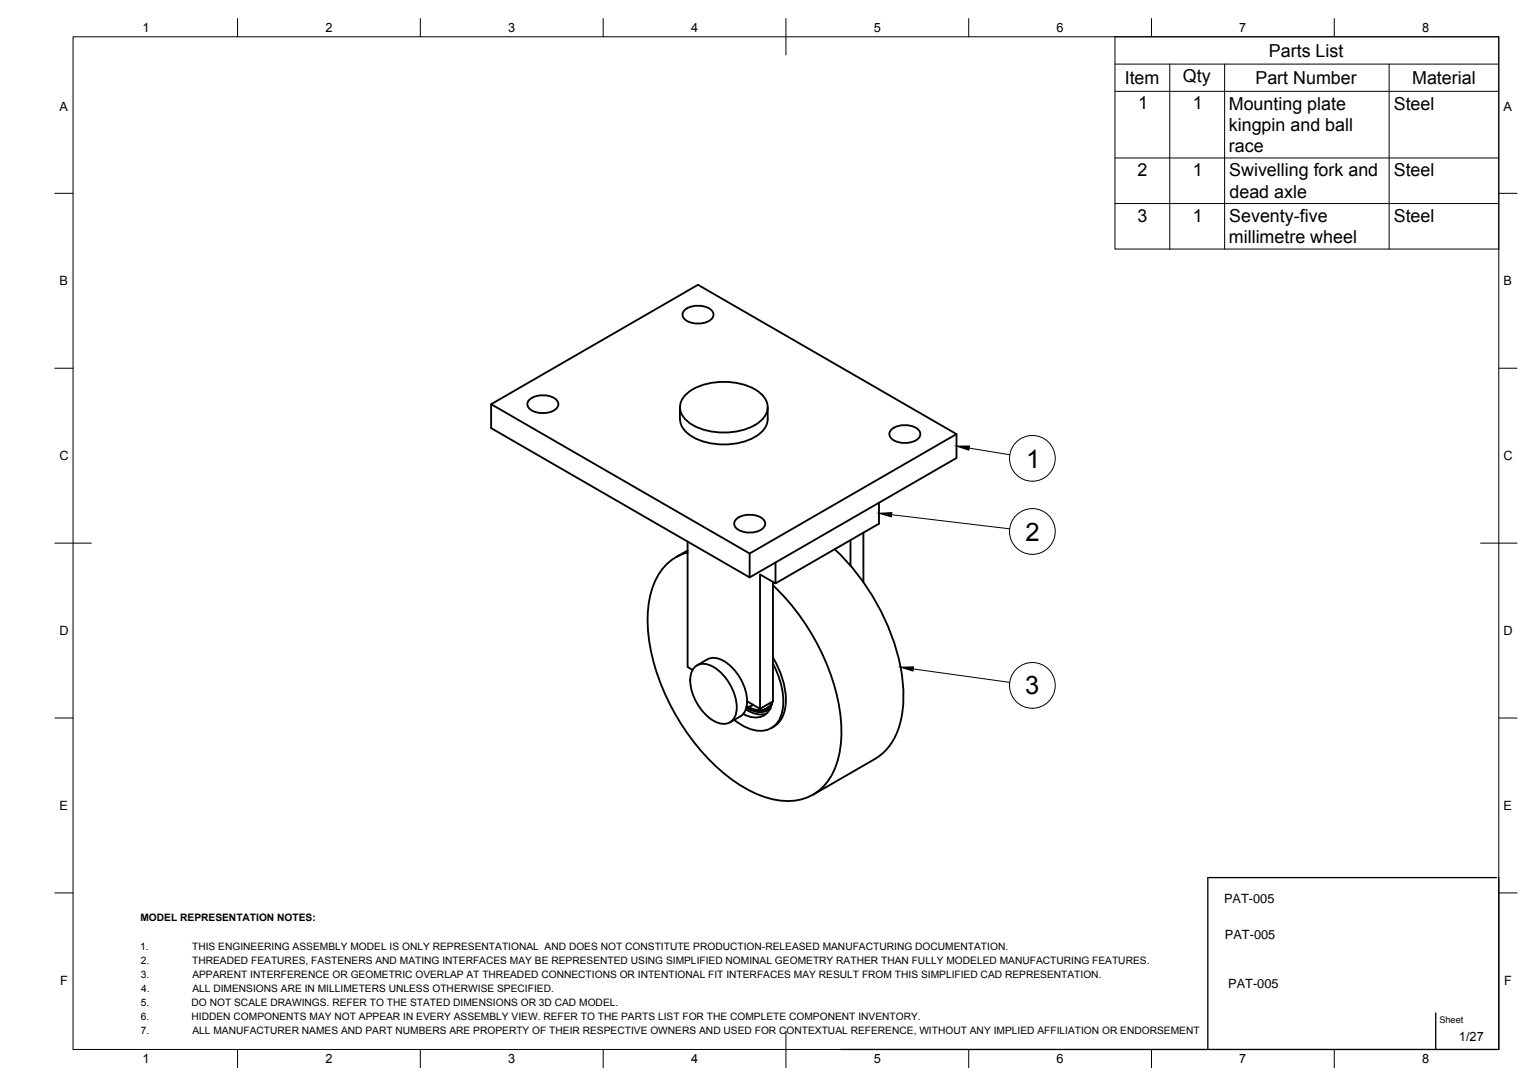
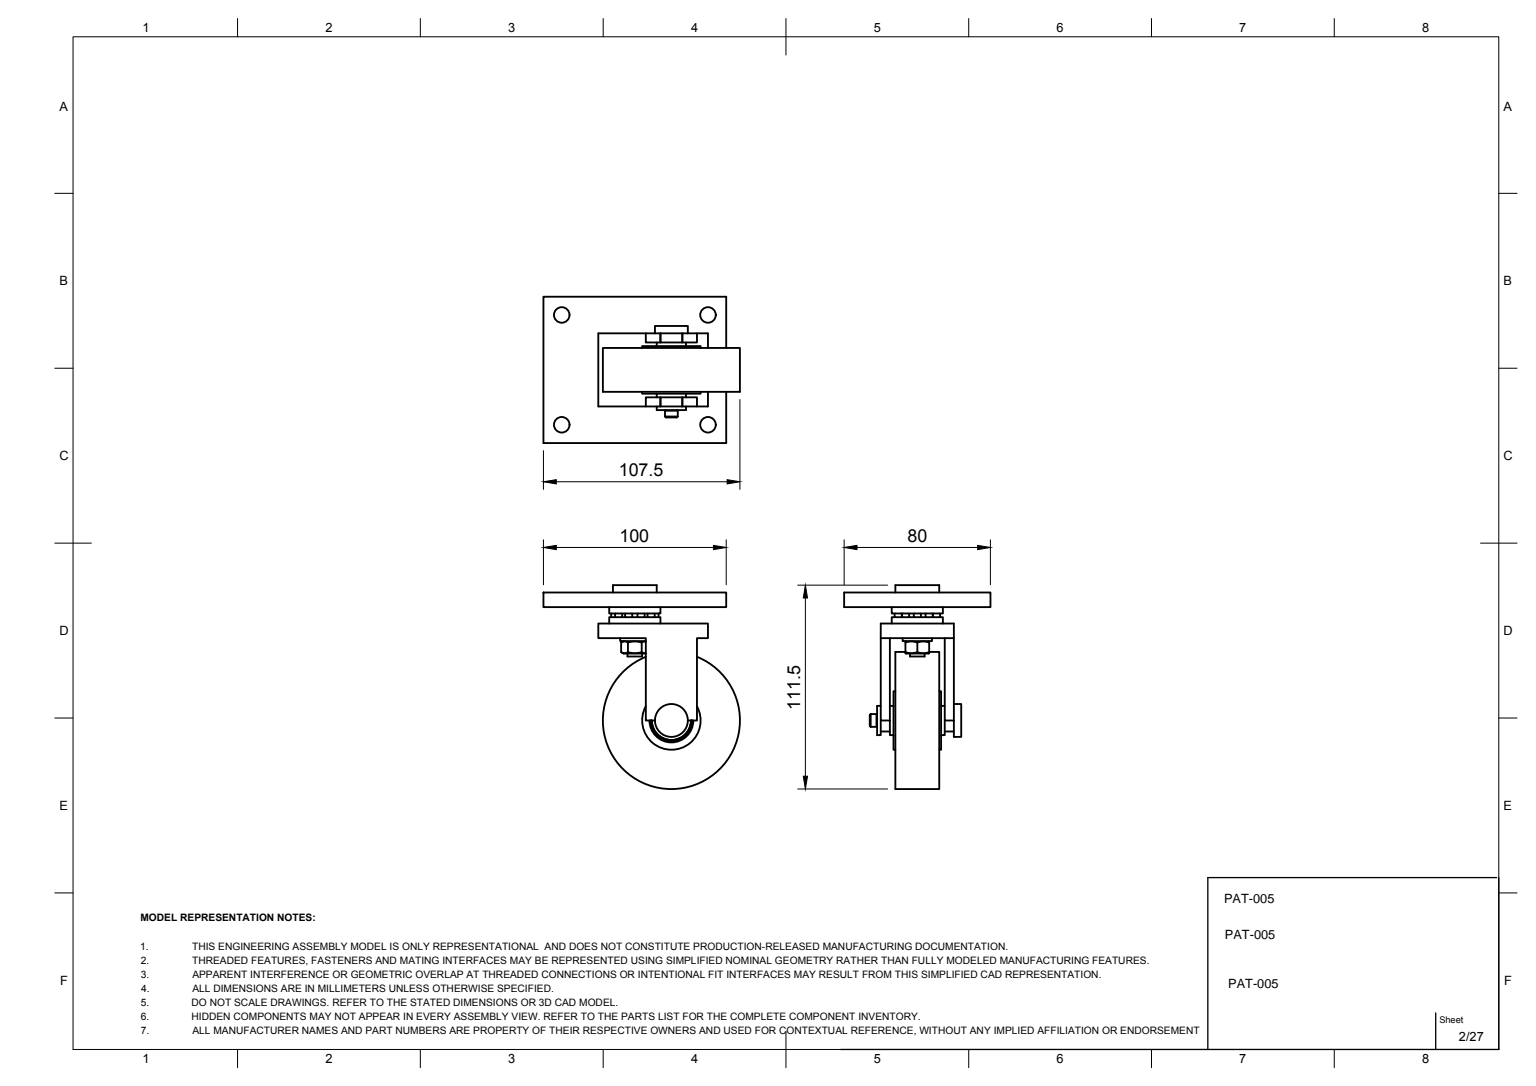
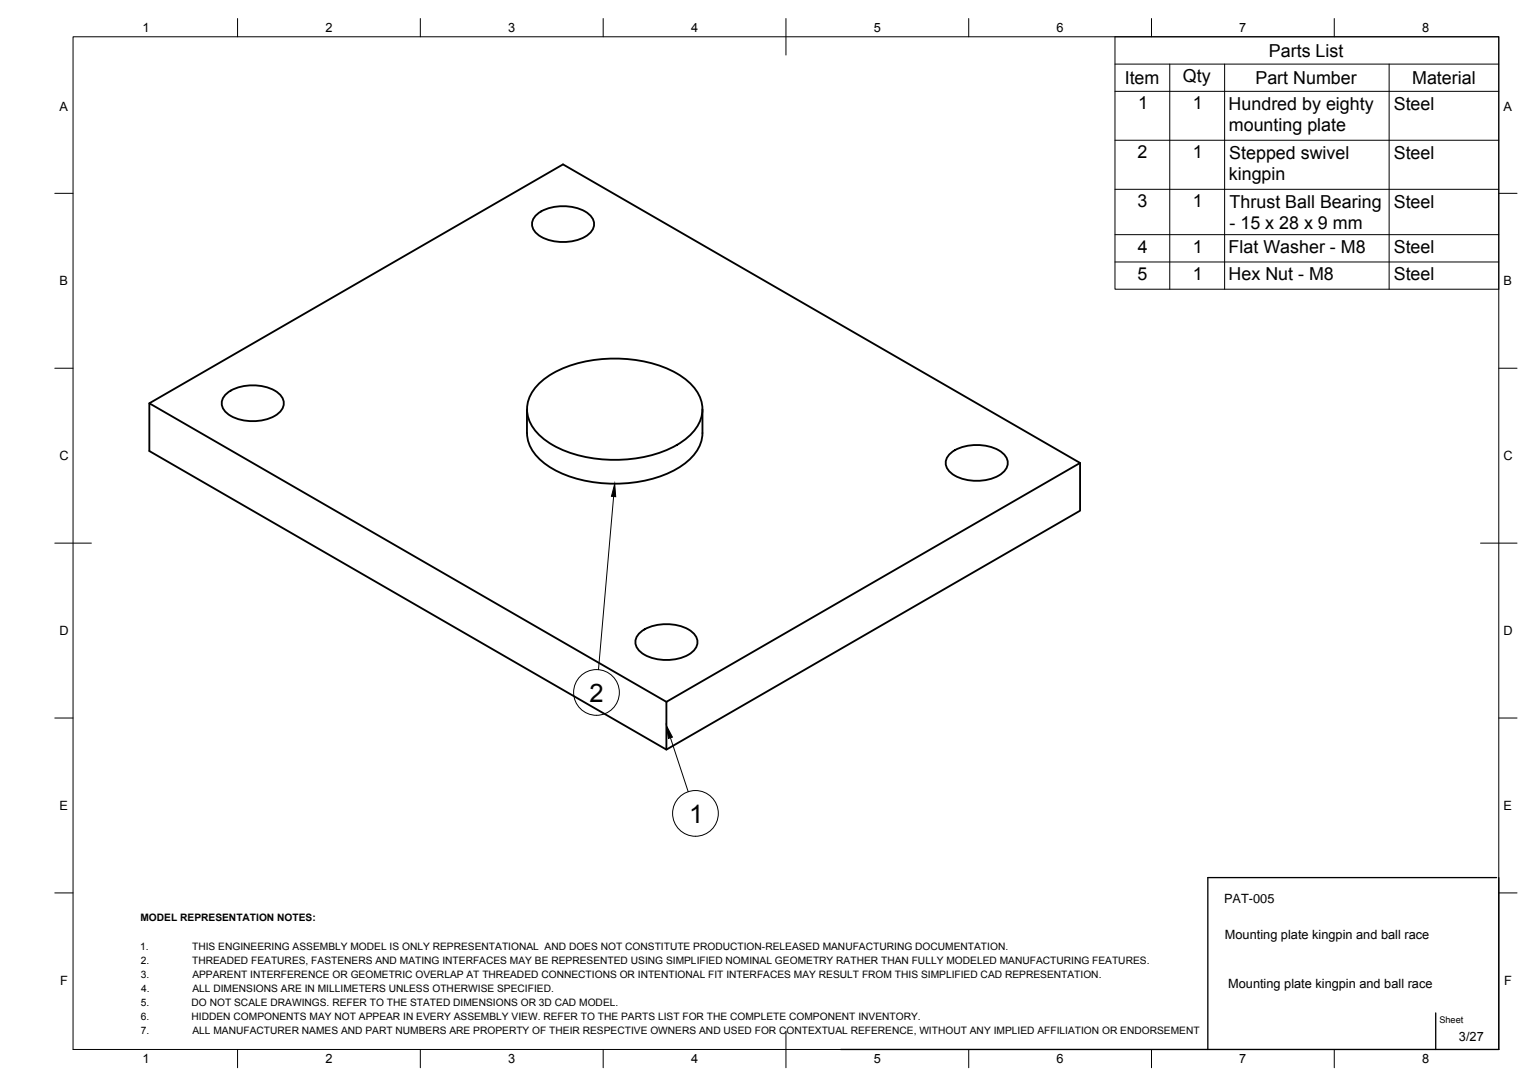
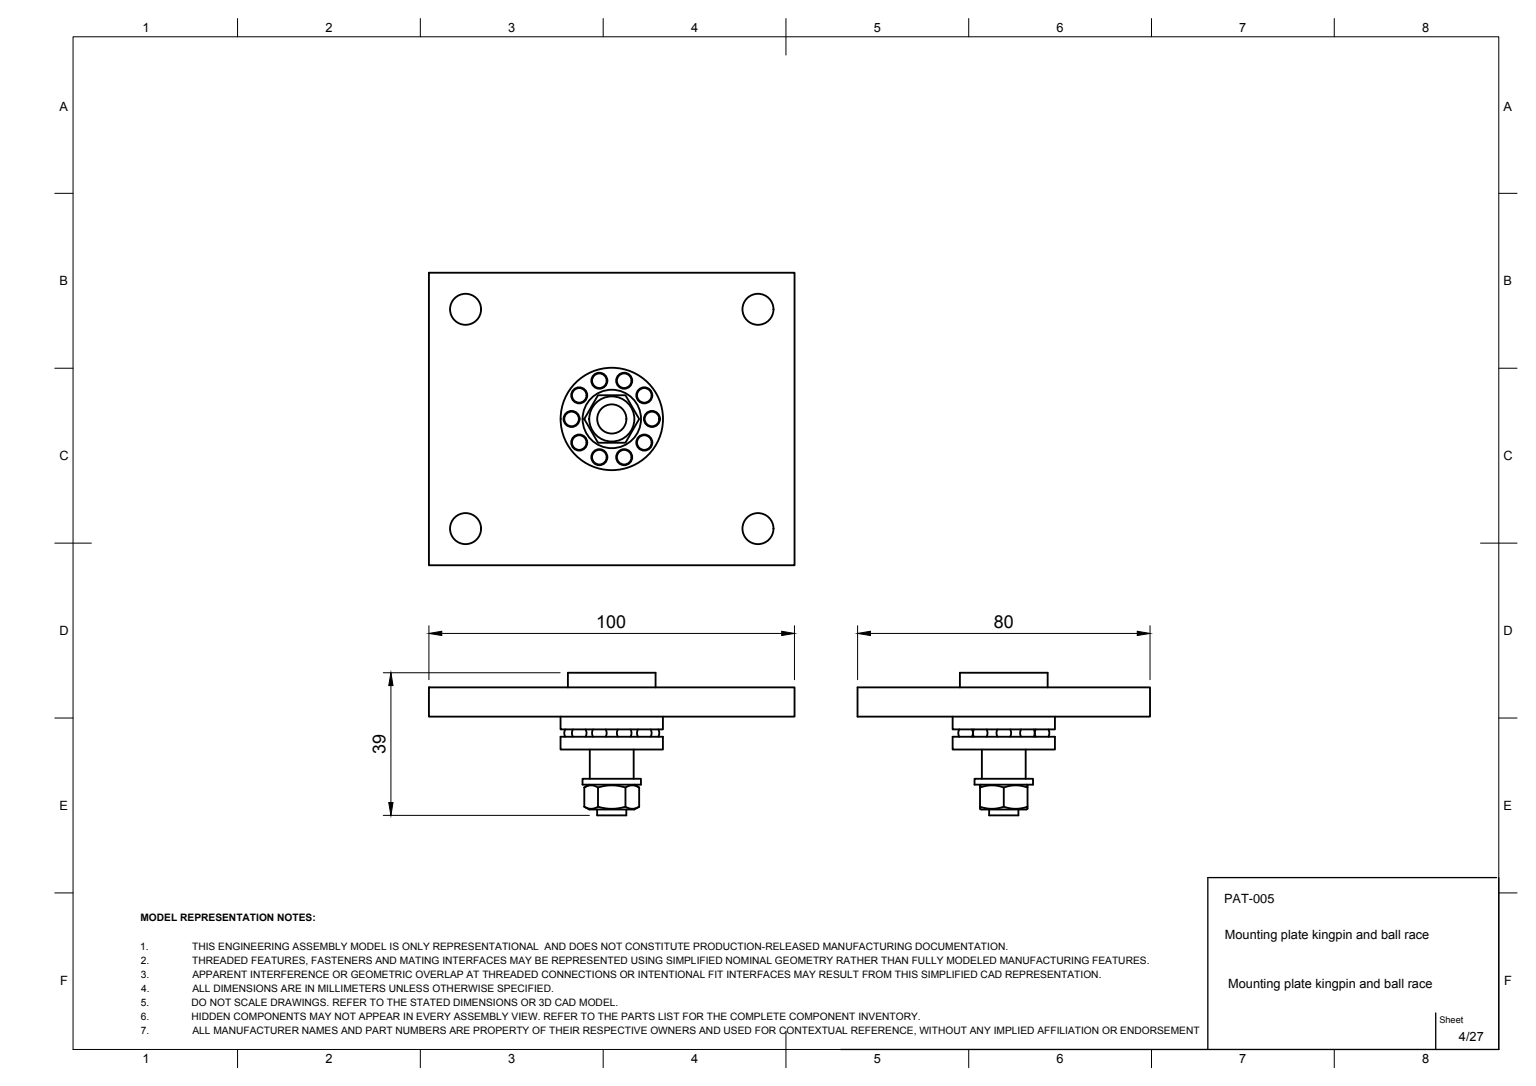
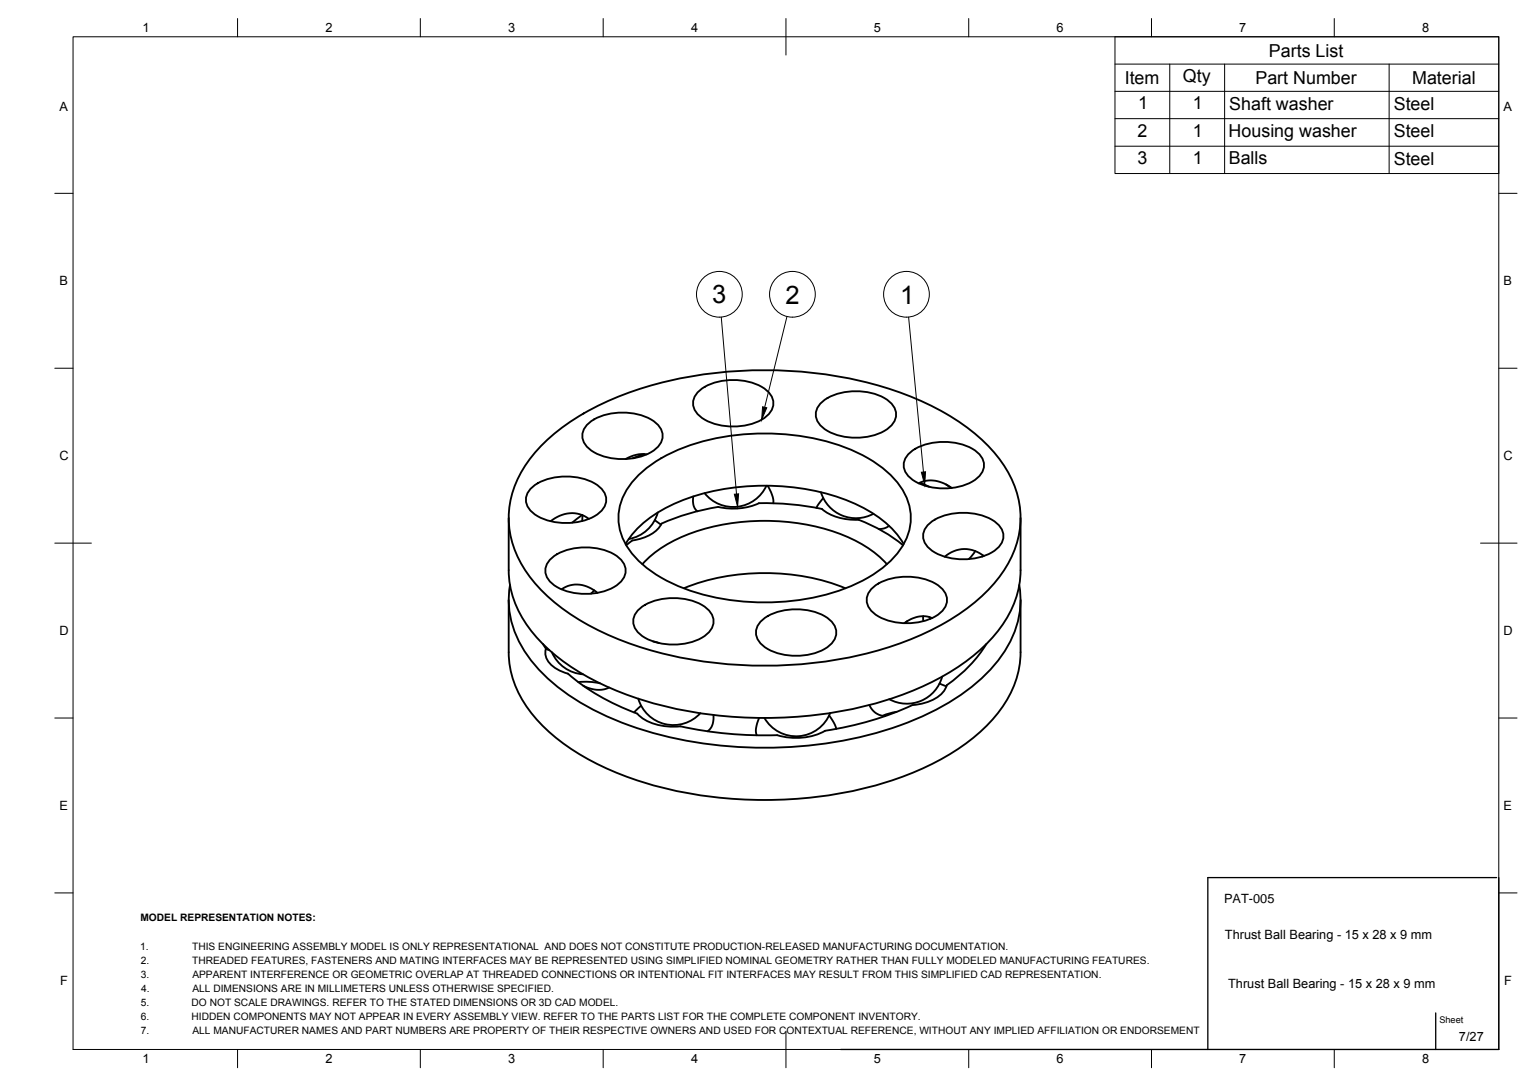
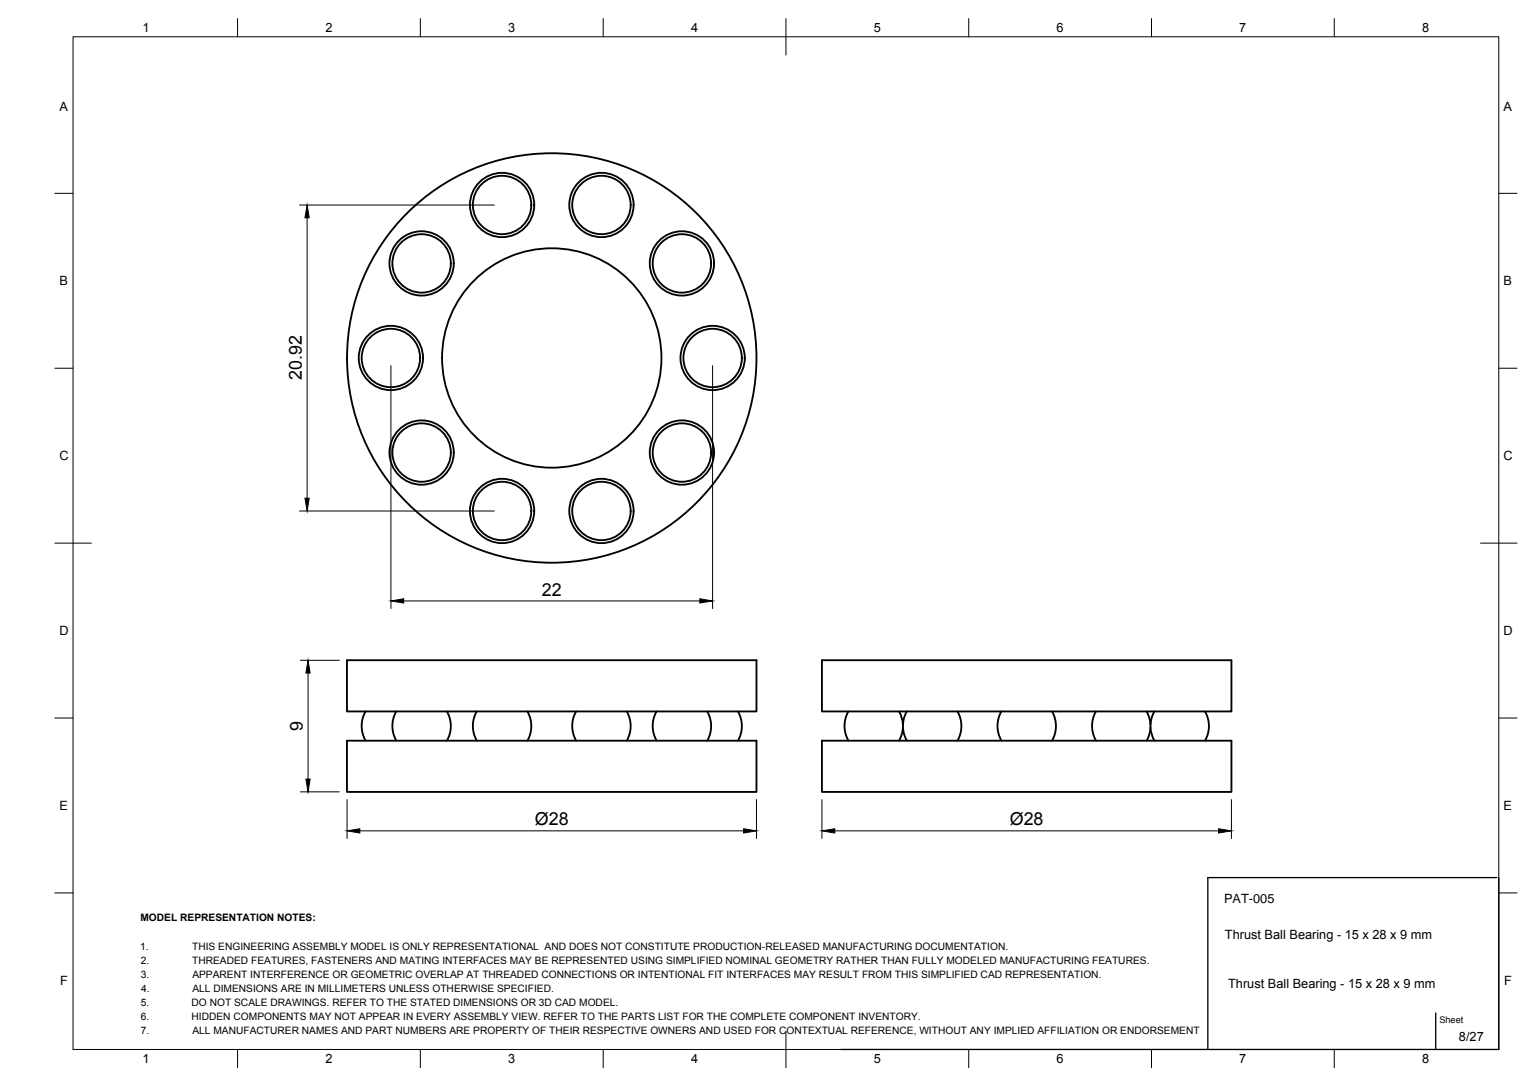
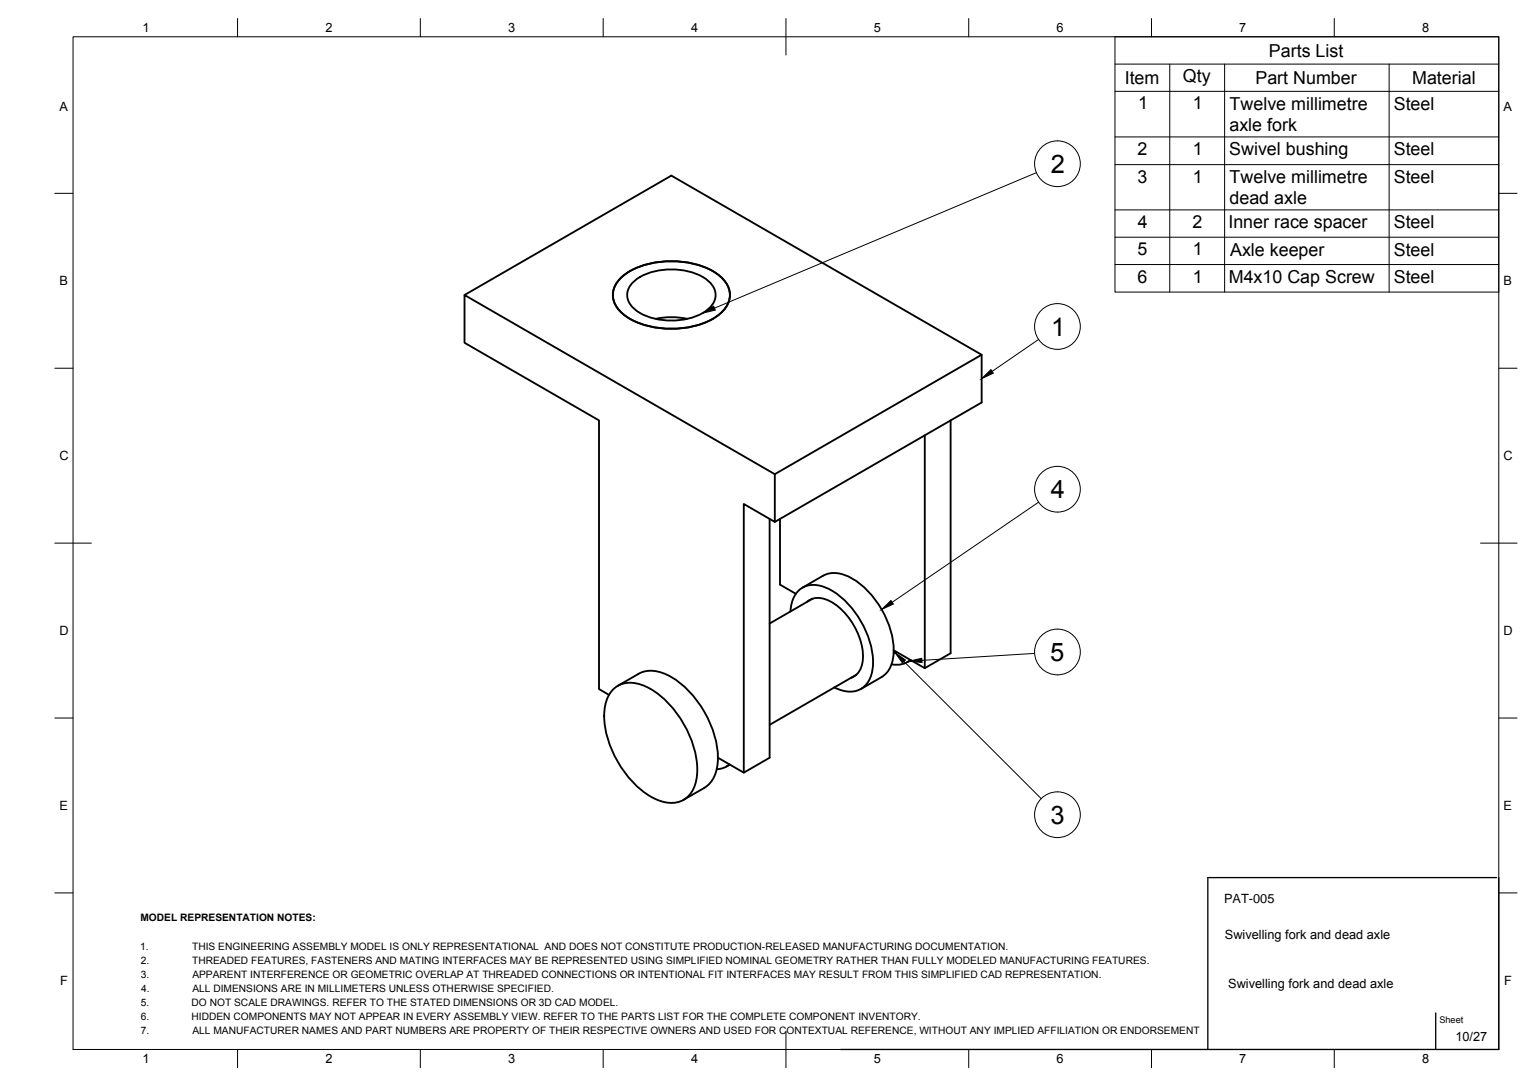
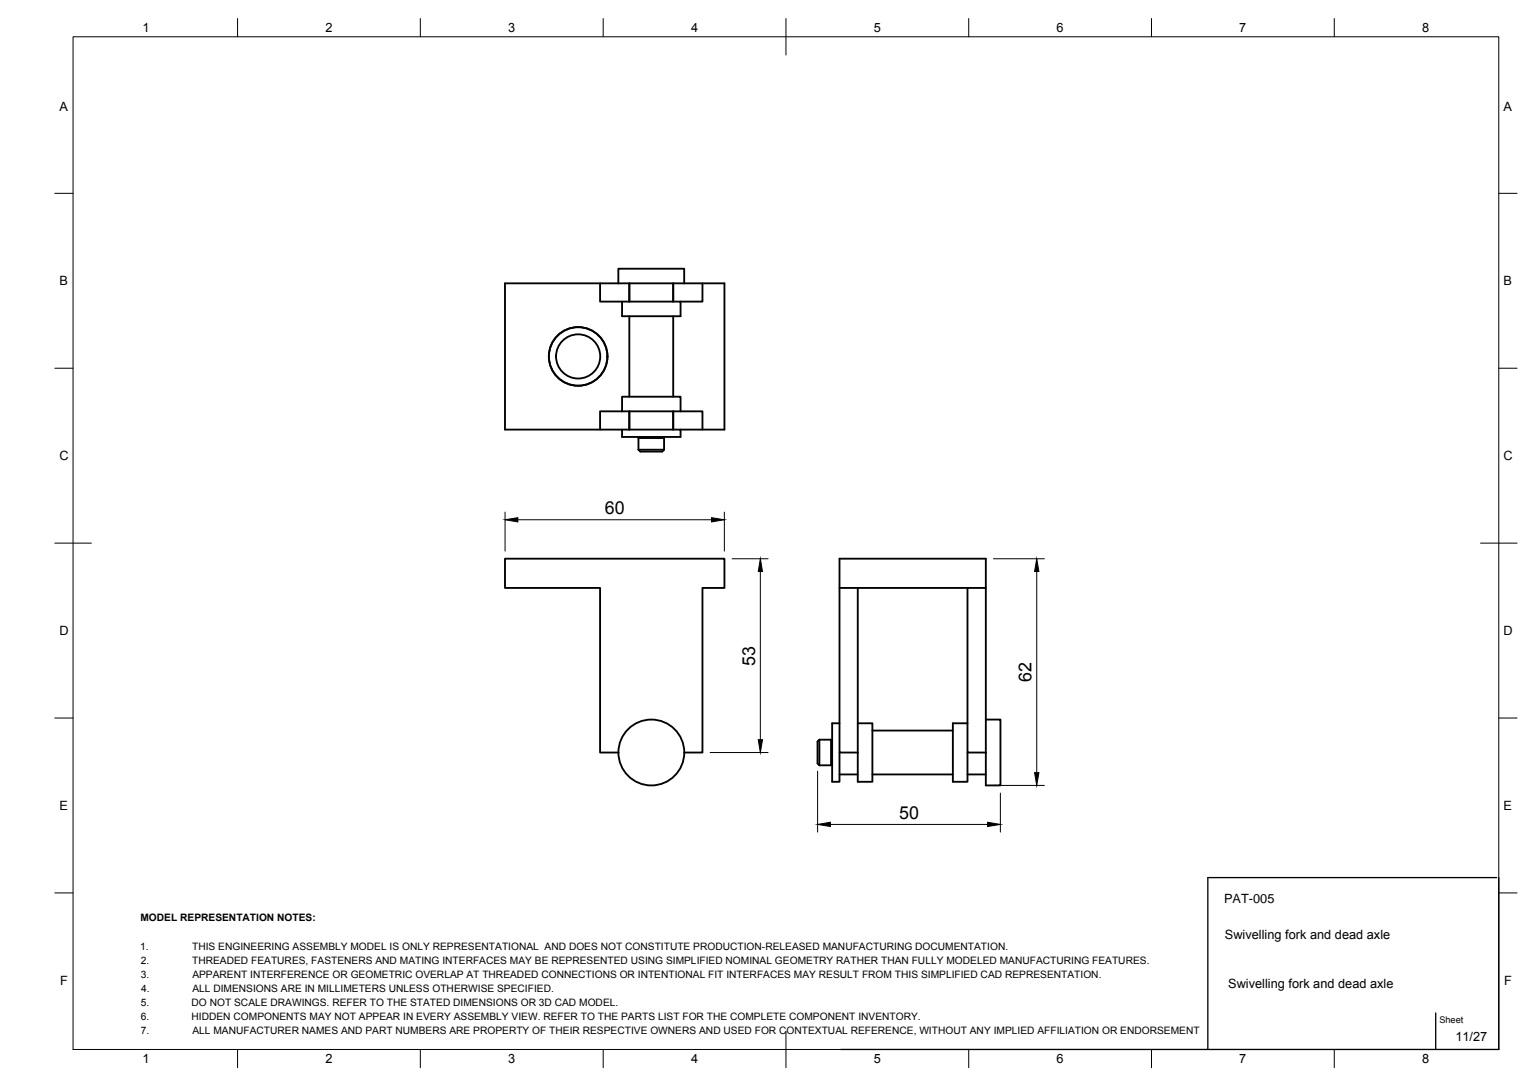
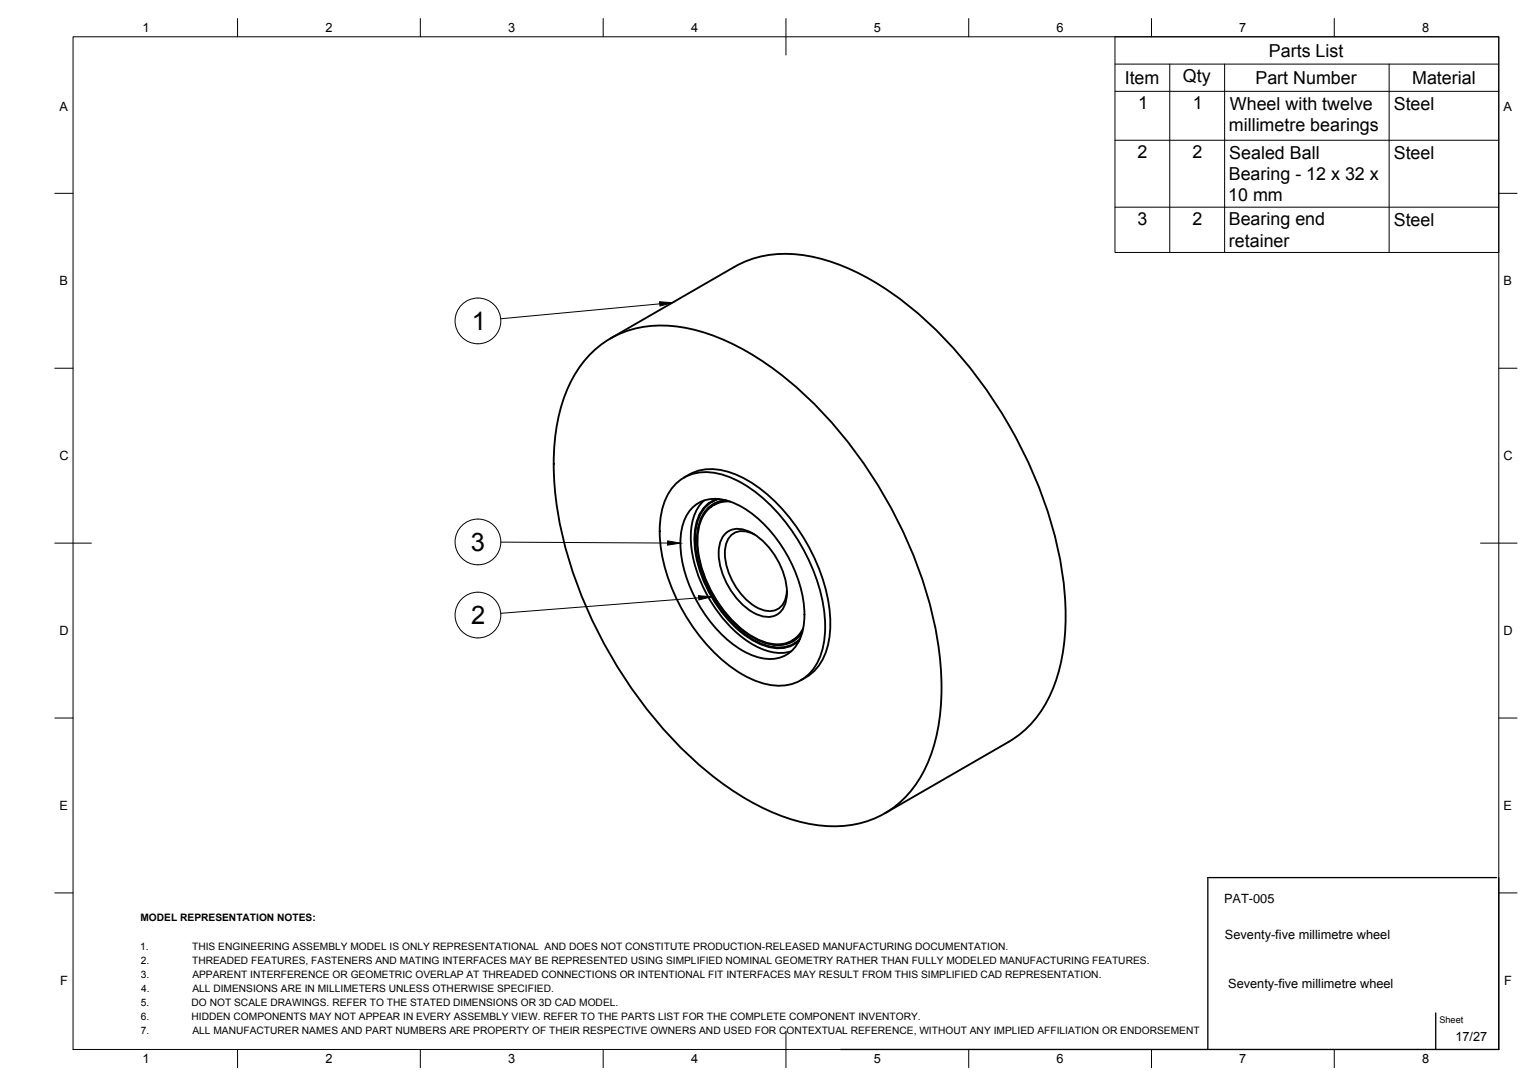
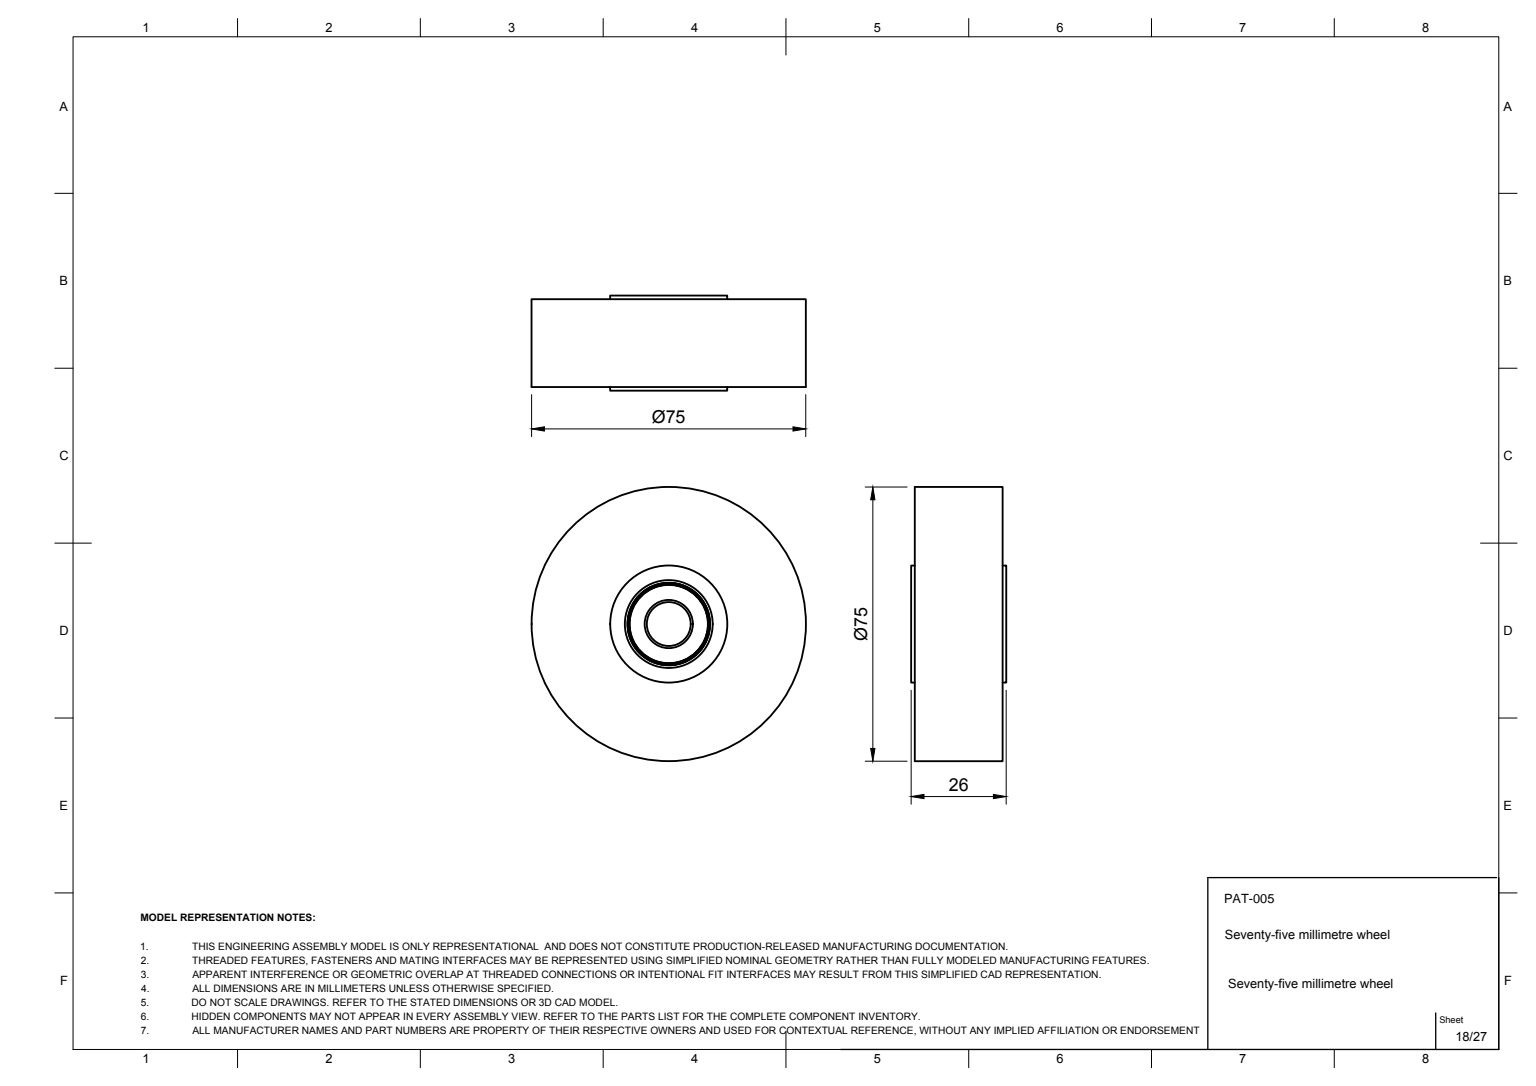
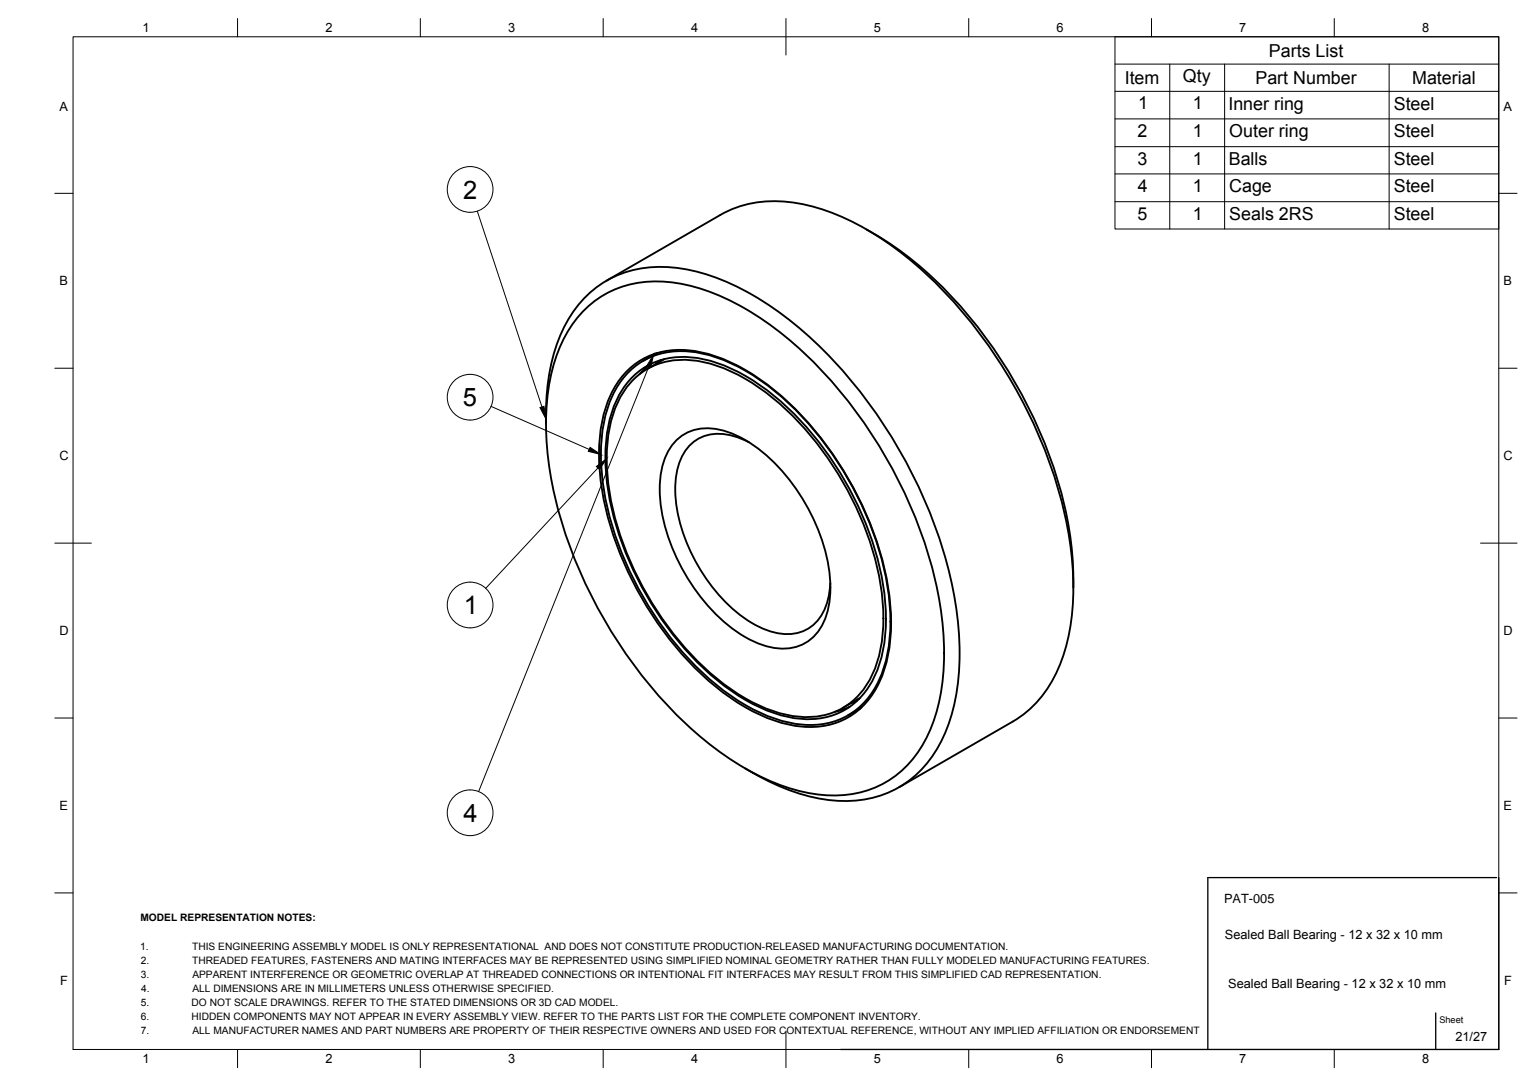
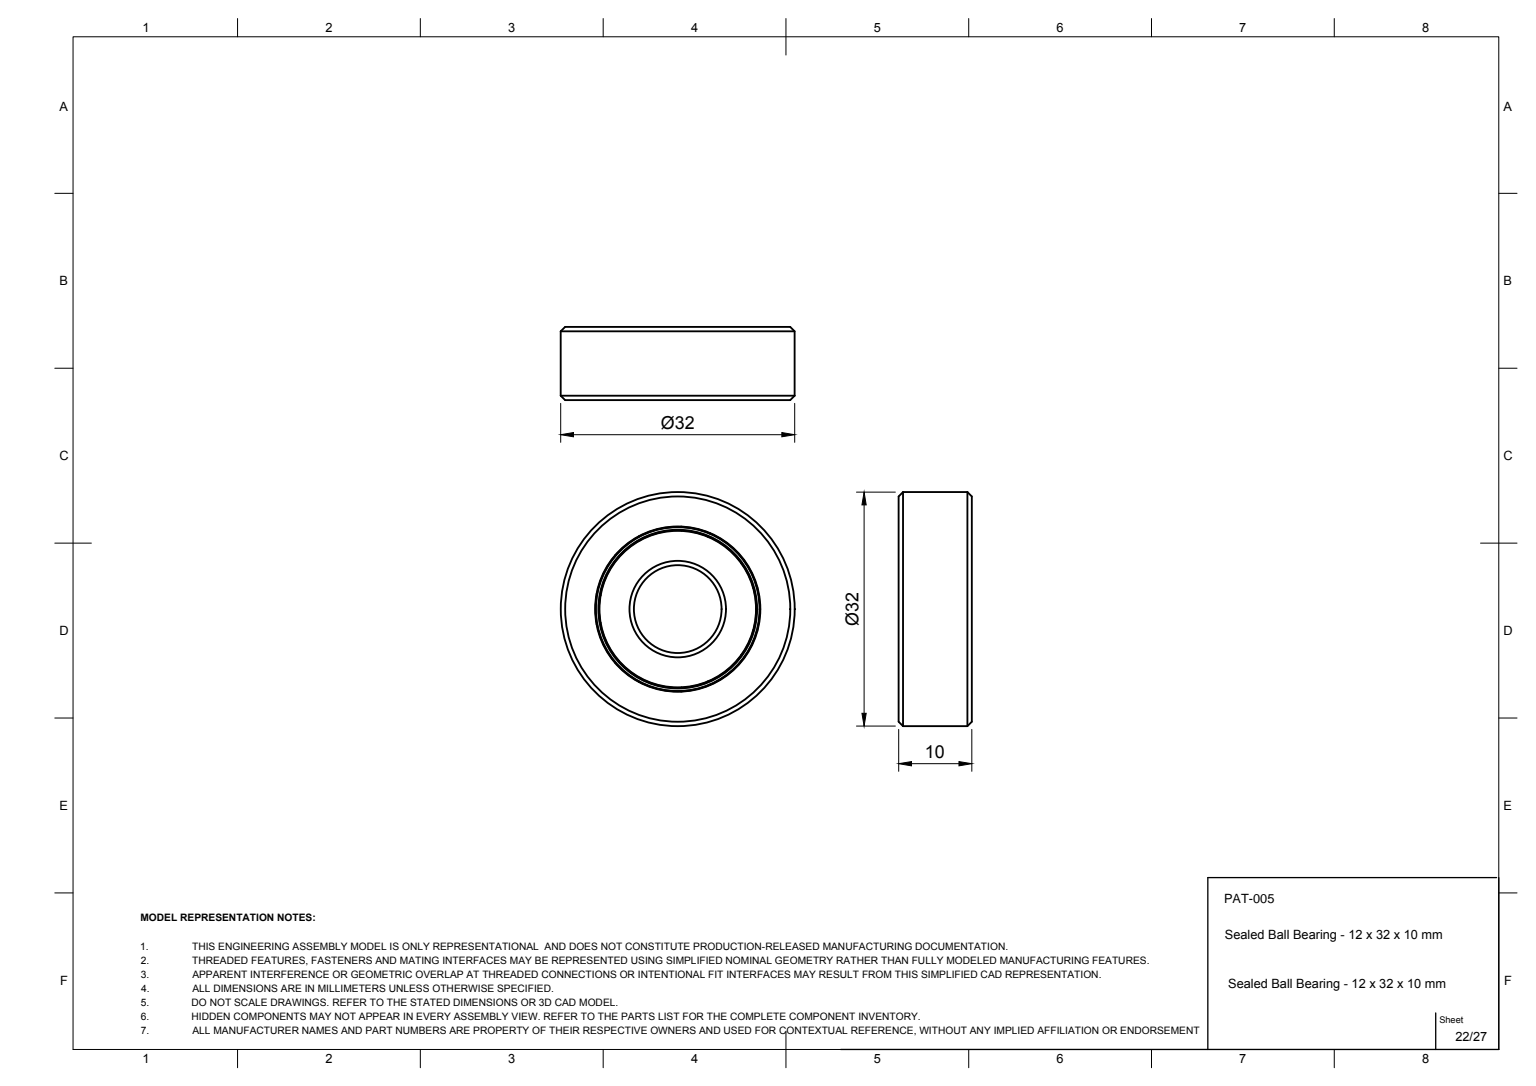
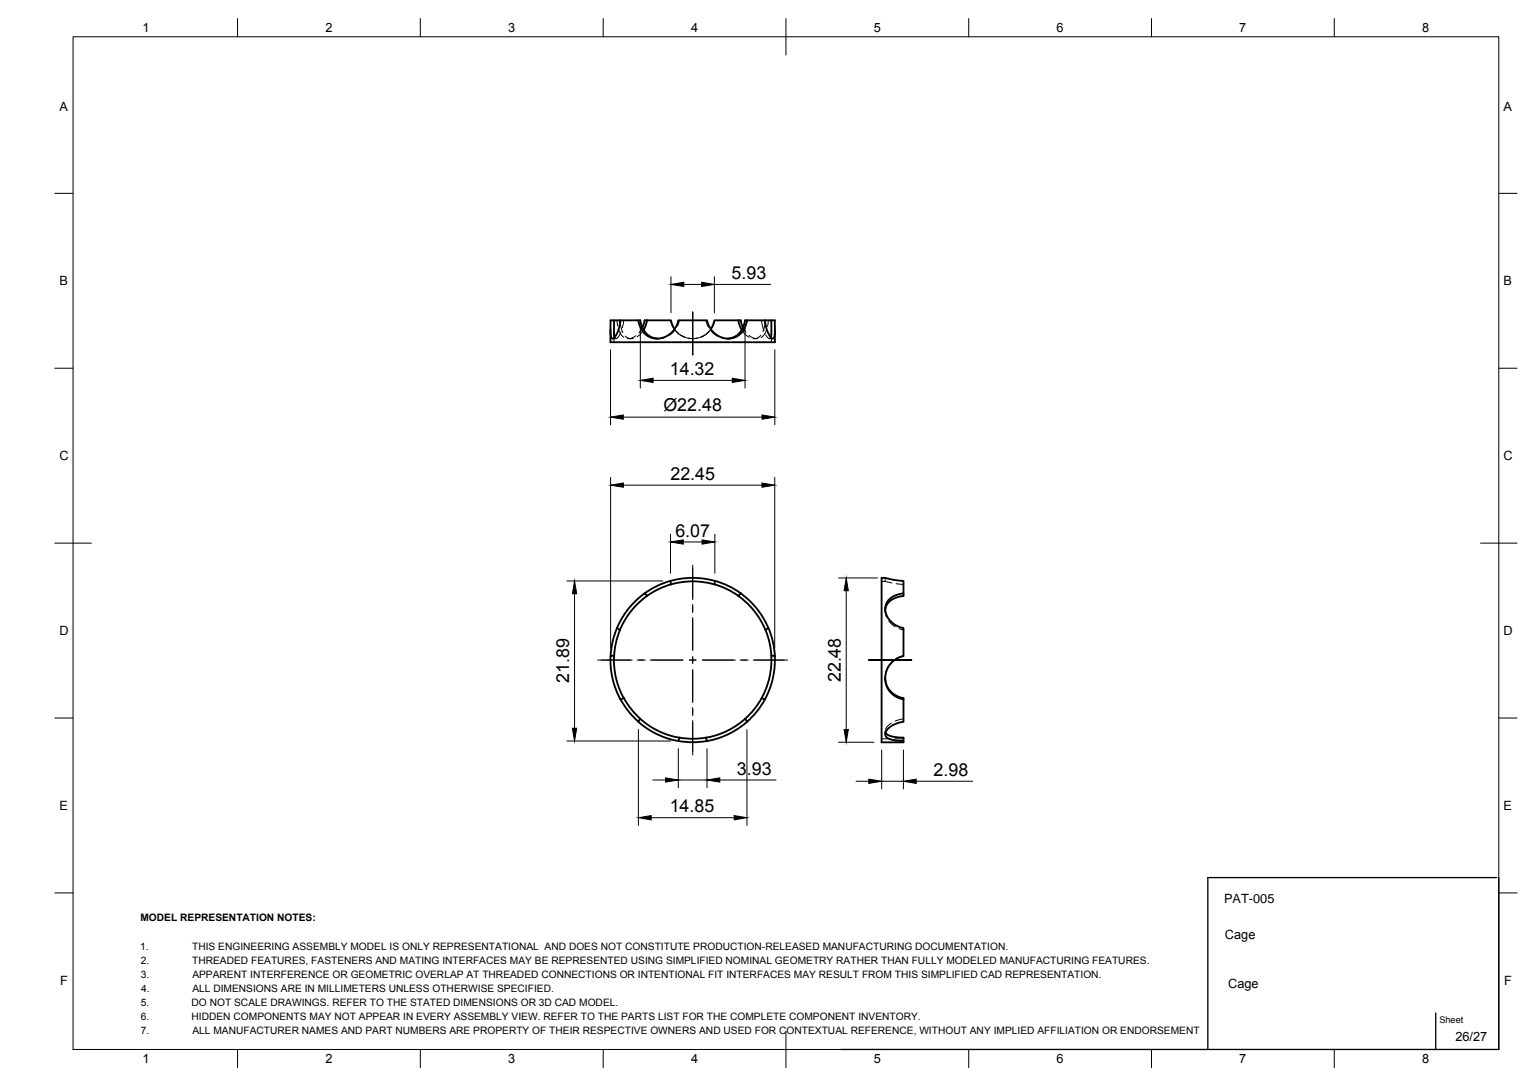
ISO-10303-21;
HEADER;
/* Generated by software containing ST-Developer
 * from STEP Tools, Inc. (www.steptools.com) 
 */

FILE_DESCRIPTION(
/* description */ ('Ball-race swivel caster'),
/* implementation_level */ '2;1');

FILE_NAME(
/* name */ 'PAT-005',
/* time_stamp */ '2026-10-29T16:15:51-07:00',
/* author */ (''),
/* organization */ (''),
/* preprocessor_version */ 'ST-DEVELOPER v20.2',
/* originating_system */ 'Autodesk Translation Framework v15.17.0.0',
/* authorisation */ '');

FILE_SCHEMA (('AUTOMOTIVE_DESIGN { 1 0 10303 214 3 1 1 }'));
ENDSEC;

DATA;
#10=MECHANICAL_DESIGN_GEOMETRIC_PRESENTATION_REPRESENTATION('',(#298,#299,
#300,#301,#302,#303,#304,#305,#306,#307,#308,#309,#310,#311,#312,#313,#314,
#315,#316,#317,#318,#319,#320,#321,#322,#323,#324,#325,#326,#327,#328,#329,
#330,#331,#332,#333),#7816);
#11=ORIENTED_CLOSED_SHELL('',*,#3725,.F.);
#12=BREP_WITH_VOIDS('Body1',#3726,(#11));
#13=(
BOUNDED_CURVE()
B_SPLINE_CURVE(2,(#6859,#6860,#6861),.UNSPECIFIED.,.F.,.F.)
B_SPLINE_CURVE_WITH_KNOTS((3,3),(0.14973948338295,0.97160236658079),
 .UNSPECIFIED.)
CURVE()
GEOMETRIC_REPRESENTATION_ITEM()
RATIONAL_B_SPLINE_CURVE((1.07140024848292,1.23714644374248,1.07140024848292))
REPRESENTATION_ITEM('')
);
#14=(
BOUNDED_CURVE()
B_SPLINE_CURVE(2,(#6863,#6864,#6865),.UNSPECIFIED.,.F.,.F.)
B_SPLINE_CURVE_WITH_KNOTS((3,3),(0.14973948338295,0.971602366580789),
 .UNSPECIFIED.)
CURVE()
GEOMETRIC_REPRESENTATION_ITEM()
RATIONAL_B_SPLINE_CURVE((1.07140024848292,1.23714644374248,1.07140024848292))
REPRESENTATION_ITEM('')
);
#15=(
BOUNDED_CURVE()
B_SPLINE_CURVE(2,(#6870,#6871,#6872),.UNSPECIFIED.,.F.,.F.)
B_SPLINE_CURVE_WITH_KNOTS((3,3),(0.14973948338295,0.97160236658079),
 .UNSPECIFIED.)
CURVE()
GEOMETRIC_REPRESENTATION_ITEM()
RATIONAL_B_SPLINE_CURVE((1.07140024848292,1.23714644374248,1.07140024848292))
REPRESENTATION_ITEM('')
);
#16=(
BOUNDED_CURVE()
B_SPLINE_CURVE(2,(#6874,#6875,#6876),.UNSPECIFIED.,.F.,.F.)
B_SPLINE_CURVE_WITH_KNOTS((3,3),(0.14973948338295,0.97160236658079),
 .UNSPECIFIED.)
CURVE()
GEOMETRIC_REPRESENTATION_ITEM()
RATIONAL_B_SPLINE_CURVE((1.07140024848292,1.23714644374248,1.07140024848292))
REPRESENTATION_ITEM('')
);
#17=(
BOUNDED_CURVE()
B_SPLINE_CURVE(2,(#6878,#6879,#6880),.UNSPECIFIED.,.F.,.F.)
B_SPLINE_CURVE_WITH_KNOTS((3,3),(0.14973948338295,0.971602366580789),
 .UNSPECIFIED.)
CURVE()
GEOMETRIC_REPRESENTATION_ITEM()
RATIONAL_B_SPLINE_CURVE((1.07140024848292,1.23714644374248,1.07140024848292))
REPRESENTATION_ITEM('')
);
#18=(
BOUNDED_CURVE()
B_SPLINE_CURVE(2,(#6881,#6882,#6883),.UNSPECIFIED.,.F.,.F.)
B_SPLINE_CURVE_WITH_KNOTS((3,3),(0.14973948338295,0.97160236658079),
 .UNSPECIFIED.)
CURVE()
GEOMETRIC_REPRESENTATION_ITEM()
RATIONAL_B_SPLINE_CURVE((1.07140024848292,1.23714644374248,1.07140024848292))
REPRESENTATION_ITEM('')
);
#19=(
BOUNDED_CURVE()
B_SPLINE_CURVE(2,(#6890,#6891,#6892),.UNSPECIFIED.,.F.,.F.)
B_SPLINE_CURVE_WITH_KNOTS((3,3),(0.14973948338295,0.97160236658079),
 .UNSPECIFIED.)
CURVE()
GEOMETRIC_REPRESENTATION_ITEM()
RATIONAL_B_SPLINE_CURVE((1.07140024848292,1.23714644374248,1.07140024848292))
REPRESENTATION_ITEM('')
);
#20=(
BOUNDED_CURVE()
B_SPLINE_CURVE(2,(#6894,#6895,#6896),.UNSPECIFIED.,.F.,.F.)
B_SPLINE_CURVE_WITH_KNOTS((3,3),(0.14973948338295,0.97160236658079),
 .UNSPECIFIED.)
CURVE()
GEOMETRIC_REPRESENTATION_ITEM()
RATIONAL_B_SPLINE_CURVE((1.07140024848292,1.23714644374248,1.07140024848292))
REPRESENTATION_ITEM('')
);
#21=(
BOUNDED_CURVE()
B_SPLINE_CURVE(2,(#6898,#6899,#6900),.UNSPECIFIED.,.F.,.F.)
B_SPLINE_CURVE_WITH_KNOTS((3,3),(0.14973948338295,0.971602366580789),
 .UNSPECIFIED.)
CURVE()
GEOMETRIC_REPRESENTATION_ITEM()
RATIONAL_B_SPLINE_CURVE((1.07140024848292,1.23714644374248,1.07140024848292))
REPRESENTATION_ITEM('')
);
#22=(
BOUNDED_CURVE()
B_SPLINE_CURVE(2,(#6902,#6903,#6904),.UNSPECIFIED.,.F.,.F.)
B_SPLINE_CURVE_WITH_KNOTS((3,3),(0.14973948338295,0.97160236658079),
 .UNSPECIFIED.)
CURVE()
GEOMETRIC_REPRESENTATION_ITEM()
RATIONAL_B_SPLINE_CURVE((1.07140024848292,1.23714644374248,1.07140024848292))
REPRESENTATION_ITEM('')
);
#23=(
BOUNDED_CURVE()
B_SPLINE_CURVE(2,(#6906,#6907,#6908),.UNSPECIFIED.,.F.,.F.)
B_SPLINE_CURVE_WITH_KNOTS((3,3),(0.14973948338295,0.97160236658079),
 .UNSPECIFIED.)
CURVE()
GEOMETRIC_REPRESENTATION_ITEM()
RATIONAL_B_SPLINE_CURVE((1.07140024848292,1.23714644374248,1.07140024848292))
REPRESENTATION_ITEM('')
);
#24=(
BOUNDED_CURVE()
B_SPLINE_CURVE(2,(#6909,#6910,#6911),.UNSPECIFIED.,.F.,.F.)
B_SPLINE_CURVE_WITH_KNOTS((3,3),(0.14973948338295,0.971602366580789),
 .UNSPECIFIED.)
CURVE()
GEOMETRIC_REPRESENTATION_ITEM()
RATIONAL_B_SPLINE_CURVE((1.07140024848292,1.23714644374248,1.07140024848292))
REPRESENTATION_ITEM('')
);
#25=CONICAL_SURFACE('',#4207,0.734027674973257,1.0471975511966);
#26=CONICAL_SURFACE('',#4209,0.734027674973257,1.0471975511966);
#27=CONICAL_SURFACE('',#4308,0.325,0.785398163397448);
#28=CONICAL_SURFACE('',#4312,0.335,0.785398163397448);
#29=CONICAL_SURFACE('',#4316,0.21,0.463647609000806);
#30=CONICAL_SURFACE('',#4357,0.63,0.785398163397448);
#31=CONICAL_SURFACE('',#4364,0.63,0.785398163397448);
#32=CONICAL_SURFACE('',#4377,1.57,0.785398163397449);
#33=CONICAL_SURFACE('',#4381,1.57,0.785398163397449);
#34=ITEM_DEFINED_TRANSFORMATION($,$,#4005,#4194);
#35=ITEM_DEFINED_TRANSFORMATION($,$,#4089,#4195);
#36=ITEM_DEFINED_TRANSFORMATION($,$,#4173,#4196);
#37=ITEM_DEFINED_TRANSFORMATION($,$,#3964,#4222);
#38=ITEM_DEFINED_TRANSFORMATION($,$,#3986,#4223);
#39=ITEM_DEFINED_TRANSFORMATION($,$,#4004,#4224);
#40=ITEM_DEFINED_TRANSFORMATION($,$,#4197,#4225);
#41=ITEM_DEFINED_TRANSFORMATION($,$,#4206,#4226);
#42=ITEM_DEFINED_TRANSFORMATION($,$,#4228,#4319);
#43=ITEM_DEFINED_TRANSFORMATION($,$,#4254,#4320);
#44=ITEM_DEFINED_TRANSFORMATION($,$,#4263,#4321);
#45=ITEM_DEFINED_TRANSFORMATION($,$,#4277,#4322);
#46=ITEM_DEFINED_TRANSFORMATION($,$,#4277,#4323);
#47=ITEM_DEFINED_TRANSFORMATION($,$,#4286,#4324);
#48=ITEM_DEFINED_TRANSFORMATION($,$,#4295,#4325);
#49=ITEM_DEFINED_TRANSFORMATION($,$,#4345,#4467);
#50=ITEM_DEFINED_TRANSFORMATION($,$,#4365,#4468);
#51=ITEM_DEFINED_TRANSFORMATION($,$,#4385,#4469);
#52=ITEM_DEFINED_TRANSFORMATION($,$,#4400,#4470);
#53=ITEM_DEFINED_TRANSFORMATION($,$,#4450,#4471);
#54=ITEM_DEFINED_TRANSFORMATION($,$,#4327,#4481);
#55=ITEM_DEFINED_TRANSFORMATION($,$,#4344,#4482);
#56=ITEM_DEFINED_TRANSFORMATION($,$,#4344,#4483);
#57=ITEM_DEFINED_TRANSFORMATION($,$,#4472,#4484);
#58=ITEM_DEFINED_TRANSFORMATION($,$,#4472,#4485);
#59=ITEM_DEFINED_TRANSFORMATION($,$,#3963,#4486);
#60=ITEM_DEFINED_TRANSFORMATION($,$,#4227,#4487);
#61=ITEM_DEFINED_TRANSFORMATION($,$,#4326,#4488);
#62=(
REPRESENTATION_RELATIONSHIP($,$,#7906,#7905)
REPRESENTATION_RELATIONSHIP_WITH_TRANSFORMATION(#34)
SHAPE_REPRESENTATION_RELATIONSHIP()
);
#63=(
REPRESENTATION_RELATIONSHIP($,$,#7907,#7905)
REPRESENTATION_RELATIONSHIP_WITH_TRANSFORMATION(#35)
SHAPE_REPRESENTATION_RELATIONSHIP()
);
#64=(
REPRESENTATION_RELATIONSHIP($,$,#7908,#7905)
REPRESENTATION_RELATIONSHIP_WITH_TRANSFORMATION(#36)
SHAPE_REPRESENTATION_RELATIONSHIP()
);
#65=(
REPRESENTATION_RELATIONSHIP($,$,#7903,#7902)
REPRESENTATION_RELATIONSHIP_WITH_TRANSFORMATION(#37)
SHAPE_REPRESENTATION_RELATIONSHIP()
);
#66=(
REPRESENTATION_RELATIONSHIP($,$,#7904,#7902)
REPRESENTATION_RELATIONSHIP_WITH_TRANSFORMATION(#38)
SHAPE_REPRESENTATION_RELATIONSHIP()
);
#67=(
REPRESENTATION_RELATIONSHIP($,$,#7905,#7902)
REPRESENTATION_RELATIONSHIP_WITH_TRANSFORMATION(#39)
SHAPE_REPRESENTATION_RELATIONSHIP()
);
#68=(
REPRESENTATION_RELATIONSHIP($,$,#7909,#7902)
REPRESENTATION_RELATIONSHIP_WITH_TRANSFORMATION(#40)
SHAPE_REPRESENTATION_RELATIONSHIP()
);
#69=(
REPRESENTATION_RELATIONSHIP($,$,#7910,#7902)
REPRESENTATION_RELATIONSHIP_WITH_TRANSFORMATION(#41)
SHAPE_REPRESENTATION_RELATIONSHIP()
);
#70=(
REPRESENTATION_RELATIONSHIP($,$,#7912,#7911)
REPRESENTATION_RELATIONSHIP_WITH_TRANSFORMATION(#42)
SHAPE_REPRESENTATION_RELATIONSHIP()
);
#71=(
REPRESENTATION_RELATIONSHIP($,$,#7913,#7911)
REPRESENTATION_RELATIONSHIP_WITH_TRANSFORMATION(#43)
SHAPE_REPRESENTATION_RELATIONSHIP()
);
#72=(
REPRESENTATION_RELATIONSHIP($,$,#7914,#7911)
REPRESENTATION_RELATIONSHIP_WITH_TRANSFORMATION(#44)
SHAPE_REPRESENTATION_RELATIONSHIP()
);
#73=(
REPRESENTATION_RELATIONSHIP($,$,#7915,#7911)
REPRESENTATION_RELATIONSHIP_WITH_TRANSFORMATION(#45)
SHAPE_REPRESENTATION_RELATIONSHIP()
);
#74=(
REPRESENTATION_RELATIONSHIP($,$,#7915,#7911)
REPRESENTATION_RELATIONSHIP_WITH_TRANSFORMATION(#46)
SHAPE_REPRESENTATION_RELATIONSHIP()
);
#75=(
REPRESENTATION_RELATIONSHIP($,$,#7916,#7911)
REPRESENTATION_RELATIONSHIP_WITH_TRANSFORMATION(#47)
SHAPE_REPRESENTATION_RELATIONSHIP()
);
#76=(
REPRESENTATION_RELATIONSHIP($,$,#7917,#7911)
REPRESENTATION_RELATIONSHIP_WITH_TRANSFORMATION(#48)
SHAPE_REPRESENTATION_RELATIONSHIP()
);
#77=(
REPRESENTATION_RELATIONSHIP($,$,#7921,#7920)
REPRESENTATION_RELATIONSHIP_WITH_TRANSFORMATION(#49)
SHAPE_REPRESENTATION_RELATIONSHIP()
);
#78=(
REPRESENTATION_RELATIONSHIP($,$,#7922,#7920)
REPRESENTATION_RELATIONSHIP_WITH_TRANSFORMATION(#50)
SHAPE_REPRESENTATION_RELATIONSHIP()
);
#79=(
REPRESENTATION_RELATIONSHIP($,$,#7923,#7920)
REPRESENTATION_RELATIONSHIP_WITH_TRANSFORMATION(#51)
SHAPE_REPRESENTATION_RELATIONSHIP()
);
#80=(
REPRESENTATION_RELATIONSHIP($,$,#7924,#7920)
REPRESENTATION_RELATIONSHIP_WITH_TRANSFORMATION(#52)
SHAPE_REPRESENTATION_RELATIONSHIP()
);
#81=(
REPRESENTATION_RELATIONSHIP($,$,#7925,#7920)
REPRESENTATION_RELATIONSHIP_WITH_TRANSFORMATION(#53)
SHAPE_REPRESENTATION_RELATIONSHIP()
);
#82=(
REPRESENTATION_RELATIONSHIP($,$,#7919,#7918)
REPRESENTATION_RELATIONSHIP_WITH_TRANSFORMATION(#54)
SHAPE_REPRESENTATION_RELATIONSHIP()
);
#83=(
REPRESENTATION_RELATIONSHIP($,$,#7920,#7918)
REPRESENTATION_RELATIONSHIP_WITH_TRANSFORMATION(#55)
SHAPE_REPRESENTATION_RELATIONSHIP()
);
#84=(
REPRESENTATION_RELATIONSHIP($,$,#7920,#7918)
REPRESENTATION_RELATIONSHIP_WITH_TRANSFORMATION(#56)
SHAPE_REPRESENTATION_RELATIONSHIP()
);
#85=(
REPRESENTATION_RELATIONSHIP($,$,#7926,#7918)
REPRESENTATION_RELATIONSHIP_WITH_TRANSFORMATION(#57)
SHAPE_REPRESENTATION_RELATIONSHIP()
);
#86=(
REPRESENTATION_RELATIONSHIP($,$,#7926,#7918)
REPRESENTATION_RELATIONSHIP_WITH_TRANSFORMATION(#58)
SHAPE_REPRESENTATION_RELATIONSHIP()
);
#87=(
REPRESENTATION_RELATIONSHIP($,$,#7902,#7901)
REPRESENTATION_RELATIONSHIP_WITH_TRANSFORMATION(#59)
SHAPE_REPRESENTATION_RELATIONSHIP()
);
#88=(
REPRESENTATION_RELATIONSHIP($,$,#7911,#7901)
REPRESENTATION_RELATIONSHIP_WITH_TRANSFORMATION(#60)
SHAPE_REPRESENTATION_RELATIONSHIP()
);
#89=(
REPRESENTATION_RELATIONSHIP($,$,#7918,#7901)
REPRESENTATION_RELATIONSHIP_WITH_TRANSFORMATION(#61)
SHAPE_REPRESENTATION_RELATIONSHIP()
);
#90=CONTEXT_DEPENDENT_SHAPE_REPRESENTATION(#62,#7855);
#91=CONTEXT_DEPENDENT_SHAPE_REPRESENTATION(#63,#7856);
#92=CONTEXT_DEPENDENT_SHAPE_REPRESENTATION(#64,#7857);
#93=CONTEXT_DEPENDENT_SHAPE_REPRESENTATION(#65,#7860);
#94=CONTEXT_DEPENDENT_SHAPE_REPRESENTATION(#66,#7861);
#95=CONTEXT_DEPENDENT_SHAPE_REPRESENTATION(#67,#7862);
#96=CONTEXT_DEPENDENT_SHAPE_REPRESENTATION(#68,#7863);
#97=CONTEXT_DEPENDENT_SHAPE_REPRESENTATION(#69,#7864);
#98=CONTEXT_DEPENDENT_SHAPE_REPRESENTATION(#70,#7872);
#99=CONTEXT_DEPENDENT_SHAPE_REPRESENTATION(#71,#7873);
#100=CONTEXT_DEPENDENT_SHAPE_REPRESENTATION(#72,#7874);
#101=CONTEXT_DEPENDENT_SHAPE_REPRESENTATION(#73,#7875);
#102=CONTEXT_DEPENDENT_SHAPE_REPRESENTATION(#74,#7876);
#103=CONTEXT_DEPENDENT_SHAPE_REPRESENTATION(#75,#7877);
#104=CONTEXT_DEPENDENT_SHAPE_REPRESENTATION(#76,#7878);
#105=CONTEXT_DEPENDENT_SHAPE_REPRESENTATION(#77,#7887);
#106=CONTEXT_DEPENDENT_SHAPE_REPRESENTATION(#78,#7888);
#107=CONTEXT_DEPENDENT_SHAPE_REPRESENTATION(#79,#7889);
#108=CONTEXT_DEPENDENT_SHAPE_REPRESENTATION(#80,#7890);
#109=CONTEXT_DEPENDENT_SHAPE_REPRESENTATION(#81,#7891);
#110=CONTEXT_DEPENDENT_SHAPE_REPRESENTATION(#82,#7893);
#111=CONTEXT_DEPENDENT_SHAPE_REPRESENTATION(#83,#7894);
#112=CONTEXT_DEPENDENT_SHAPE_REPRESENTATION(#84,#7895);
#113=CONTEXT_DEPENDENT_SHAPE_REPRESENTATION(#85,#7896);
#114=CONTEXT_DEPENDENT_SHAPE_REPRESENTATION(#86,#7897);
#115=CONTEXT_DEPENDENT_SHAPE_REPRESENTATION(#87,#7898);
#116=CONTEXT_DEPENDENT_SHAPE_REPRESENTATION(#88,#7899);
#117=CONTEXT_DEPENDENT_SHAPE_REPRESENTATION(#89,#7900);
#118=NEXT_ASSEMBLY_USAGE_OCCURRENCE('Shaft washer:1','Shaft washer:1',
'Shaft washer:1',#7932,#7933,'Shaft washer:1');
#119=NEXT_ASSEMBLY_USAGE_OCCURRENCE('Housing washer:1',
'Housing washer:1','Housing washer:1',#7932,#7934,'Housing washer:1');
#120=NEXT_ASSEMBLY_USAGE_OCCURRENCE('Balls:1','Balls:1','Balls:1',#7932,
#7935,'Balls:1');
#121=NEXT_ASSEMBLY_USAGE_OCCURRENCE(
'Hundred by eighty mounting plate:1',
'Hundred by eighty mounting plate:1',
'Hundred by eighty mounting plate:1',#7929,#7930,
'Hundred by eighty mounting plate:1');
#122=NEXT_ASSEMBLY_USAGE_OCCURRENCE('Stepped swivel kingpin:1',
'Stepped swivel kingpin:1','Stepped swivel kingpin:1',#7929,#7931,
'Stepped swivel kingpin:1');
#123=NEXT_ASSEMBLY_USAGE_OCCURRENCE(
'Thrust Ball Bearing - 15 x 28 x 9 mm:2',
'Thrust Ball Bearing - 15 x 28 x 9 mm:2',
'Thrust Ball Bearing - 15 x 28 x 9 mm:2',#7929,#7932,
'Thrust Ball Bearing - 15 x 28 x 9 mm:2');
#124=NEXT_ASSEMBLY_USAGE_OCCURRENCE('Flat Washer - M8:2',
'Flat Washer - M8:2','Flat Washer - M8:2',#7929,#7936,
'Flat Washer - M8:2');
#125=NEXT_ASSEMBLY_USAGE_OCCURRENCE('Hex Nut - M8:2','Hex Nut - M8:2',
'Hex Nut - M8:2',#7929,#7937,'Hex Nut - M8:2');
#126=NEXT_ASSEMBLY_USAGE_OCCURRENCE('Twelve millimetre axle fork:1',
'Twelve millimetre axle fork:1','Twelve millimetre axle fork:1',#7938,#7939,
'Twelve millimetre axle fork:1');
#127=NEXT_ASSEMBLY_USAGE_OCCURRENCE('Swivel bushing:2',
'Swivel bushing:2','Swivel bushing:2',#7938,#7940,'Swivel bushing:2');
#128=NEXT_ASSEMBLY_USAGE_OCCURRENCE('Twelve millimetre dead axle:2',
'Twelve millimetre dead axle:2','Twelve millimetre dead axle:2',#7938,#7941,
'Twelve millimetre dead axle:2');
#129=NEXT_ASSEMBLY_USAGE_OCCURRENCE('Inner race spacer:2',
'Inner race spacer:2','Inner race spacer:2',#7938,#7942,
'Inner race spacer:2');
#130=NEXT_ASSEMBLY_USAGE_OCCURRENCE('Inner race spacer:3',
'Inner race spacer:3','Inner race spacer:3',#7938,#7942,
'Inner race spacer:3');
#131=NEXT_ASSEMBLY_USAGE_OCCURRENCE('Axle keeper:2','Axle keeper:2',
'Axle keeper:2',#7938,#7943,'Axle keeper:2');
#132=NEXT_ASSEMBLY_USAGE_OCCURRENCE('M4x10 Cap Screw:2',
'M4x10 Cap Screw:2','M4x10 Cap Screw:2',#7938,#7944,'M4x10 Cap Screw:2');
#133=NEXT_ASSEMBLY_USAGE_OCCURRENCE('Inner ring:1','Inner ring:1',
'Inner ring:1',#7947,#7948,'Inner ring:1');
#134=NEXT_ASSEMBLY_USAGE_OCCURRENCE('Outer ring:1','Outer ring:1',
'Outer ring:1',#7947,#7949,'Outer ring:1');
#135=NEXT_ASSEMBLY_USAGE_OCCURRENCE('Balls (1):1','Balls (1):1',
'Balls (1):1',#7947,#7950,'Balls (1):1');
#136=NEXT_ASSEMBLY_USAGE_OCCURRENCE('Cage (1):1','Cage (1):1',
'Cage (1):1',#7947,#7951,'Cage (1):1');
#137=NEXT_ASSEMBLY_USAGE_OCCURRENCE('Seals 2RS:1','Seals 2RS:1',
'Seals 2RS:1',#7947,#7952,'Seals 2RS:1');
#138=NEXT_ASSEMBLY_USAGE_OCCURRENCE(
'Wheel with twelve millimetre bearings:2',
'Wheel with twelve millimetre bearings:2',
'Wheel with twelve millimetre bearings:2',#7945,#7946,
'Wheel with twelve millimetre bearings:2');
#139=NEXT_ASSEMBLY_USAGE_OCCURRENCE(
'Sealed Ball Bearing - 12 x 32 x 10 mm:2',
'Sealed Ball Bearing - 12 x 32 x 10 mm:2',
'Sealed Ball Bearing - 12 x 32 x 10 mm:2',#7945,#7947,
'Sealed Ball Bearing - 12 x 32 x 10 mm:2');
#140=NEXT_ASSEMBLY_USAGE_OCCURRENCE(
'Sealed Ball Bearing - 12 x 32 x 10 mm:3',
'Sealed Ball Bearing - 12 x 32 x 10 mm:3',
'Sealed Ball Bearing - 12 x 32 x 10 mm:3',#7945,#7947,
'Sealed Ball Bearing - 12 x 32 x 10 mm:3');
#141=NEXT_ASSEMBLY_USAGE_OCCURRENCE('Bearing end retainer:2',
'Bearing end retainer:2','Bearing end retainer:2',#7945,#7953,
'Bearing end retainer:2');
#142=NEXT_ASSEMBLY_USAGE_OCCURRENCE('Bearing end retainer:3',
'Bearing end retainer:3','Bearing end retainer:3',#7945,#7953,
'Bearing end retainer:3');
#143=NEXT_ASSEMBLY_USAGE_OCCURRENCE(
'Mounting plate kingpin and ball race:1',
'Mounting plate kingpin and ball race:1',
'Mounting plate kingpin and ball race:1',#7928,#7929,
'Mounting plate kingpin and ball race:1');
#144=NEXT_ASSEMBLY_USAGE_OCCURRENCE('Swivelling fork and dead axle:1',
'Swivelling fork and dead axle:1','Swivelling fork and dead axle:1',#7928,
#7938,'Swivelling fork and dead axle:1');
#145=NEXT_ASSEMBLY_USAGE_OCCURRENCE('Seventy-five millimetre wheel:1',
'Seventy-five millimetre wheel:1','Seventy-five millimetre wheel:1',#7928,
#7945,'Seventy-five millimetre wheel:1');
#146=SPHERICAL_SURFACE('',#4174,0.2);
#147=SPHERICAL_SURFACE('',#4176,0.2);
#148=SPHERICAL_SURFACE('',#4178,0.2);
#149=SPHERICAL_SURFACE('',#4180,0.2);
#150=SPHERICAL_SURFACE('',#4182,0.2);
#151=SPHERICAL_SURFACE('',#4184,0.2);
#152=SPHERICAL_SURFACE('',#4186,0.2);
#153=SPHERICAL_SURFACE('',#4188,0.2);
#154=SPHERICAL_SURFACE('',#4190,0.2);
#155=SPHERICAL_SURFACE('',#4192,0.2);
#156=SPHERICAL_SURFACE('',#4386,0.29765);
#157=SPHERICAL_SURFACE('',#4388,0.29765);
#158=SPHERICAL_SURFACE('',#4390,0.29765);
#159=SPHERICAL_SURFACE('',#4392,0.29765);
#160=SPHERICAL_SURFACE('',#4394,0.29765);
#161=SPHERICAL_SURFACE('',#4396,0.29765);
#162=SPHERICAL_SURFACE('',#4398,0.29765);
#163=SPHERICAL_SURFACE('',#4401,0.309556);
#164=SPHERICAL_SURFACE('',#4417,0.309556);
#165=SPHERICAL_SURFACE('',#4422,0.309556);
#166=SPHERICAL_SURFACE('',#4428,0.309556);
#167=SPHERICAL_SURFACE('',#4433,0.309556);
#168=SPHERICAL_SURFACE('',#4438,0.309556);
#169=SPHERICAL_SURFACE('',#4446,0.309556);
#170=TOROIDAL_SURFACE('',#4062,1.1,0.208);
#171=TOROIDAL_SURFACE('',#4064,1.1,0.208);
#172=TOROIDAL_SURFACE('',#4066,1.1,0.208);
#173=TOROIDAL_SURFACE('',#4068,1.1,0.208);
#174=TOROIDAL_SURFACE('',#4070,1.1,0.208);
#175=TOROIDAL_SURFACE('',#4072,1.1,0.208);
#176=TOROIDAL_SURFACE('',#4074,1.1,0.208);
#177=TOROIDAL_SURFACE('',#4076,1.1,0.208);
#178=TOROIDAL_SURFACE('',#4078,1.1,0.208);
#179=TOROIDAL_SURFACE('',#4080,1.1,0.208);
#180=TOROIDAL_SURFACE('',#4146,1.1,0.208);
#181=TOROIDAL_SURFACE('',#4148,1.1,0.208);
#182=TOROIDAL_SURFACE('',#4150,1.1,0.208);
#183=TOROIDAL_SURFACE('',#4152,1.1,0.208);
#184=TOROIDAL_SURFACE('',#4154,1.1,0.208);
#185=TOROIDAL_SURFACE('',#4156,1.1,0.208);
#186=TOROIDAL_SURFACE('',#4158,1.1,0.208);
#187=TOROIDAL_SURFACE('',#4160,1.1,0.208);
#188=TOROIDAL_SURFACE('',#4162,1.1,0.208);
#189=TOROIDAL_SURFACE('',#4164,1.1,0.208);
#190=TOROIDAL_SURFACE('',#4346,1.1,0.309556);
#191=TOROIDAL_SURFACE('',#4366,1.1,0.309556);
#192=B_SPLINE_CURVE_WITH_KNOTS('',3,(#5795,#5796,#5797,#5798,#5799,#5800,
#5801,#5802,#5803,#5804),.UNSPECIFIED.,.F.,.F.,(4,2,2,2,4),(-0.464072133285151,
-0.409463462974798,-0.35465357795961,-0.295254131517933,-0.285596349669134),
 .UNSPECIFIED.);
#193=B_SPLINE_CURVE_WITH_KNOTS('',3,(#5808,#5809,#5810,#5811,#5812,#5813,
#5814,#5815,#5816,#5817,#5818,#5819,#5820,#5821,#5822,#5823),
 .UNSPECIFIED.,.F.,.F.,(4,2,2,2,2,2,2,4),(-0.45417904189248,-0.395759356749822,
-0.338728191012566,-0.275894647345884,-0.221135020913429,-0.164911408034045,
-0.0984111283989842,0.),.UNSPECIFIED.);
#194=B_SPLINE_CURVE_WITH_KNOTS('',3,(#5826,#5827,#5828,#5829,#5830,#5831,
#5832,#5833,#5834,#5835),.UNSPECIFIED.,.F.,.F.,(4,2,2,2,4),(-0.285596349669134,
-0.239649525441968,-0.179869516594422,-0.105654793183186,0.),
 .UNSPECIFIED.);
#195=B_SPLINE_CURVE_WITH_KNOTS('',3,(#5844,#5845,#5846,#5847,#5848,#5849,
#5850,#5851,#5852,#5853,#5854,#5855,#5856,#5857,#5858,#5859),
 .UNSPECIFIED.,.F.,.F.,(4,2,2,2,2,2,2,4),(-0.464097123055984,-0.409448749757932,
-0.354953921831336,-0.295351891164135,-0.239773021090731,-0.179990573569022,
-0.105700836781513,0.),.UNSPECIFIED.);
#196=B_SPLINE_CURVE_WITH_KNOTS('',3,(#5863,#5864,#5865,#5866,#5867,#5868,
#5869,#5870,#5871,#5872,#5873,#5874,#5875,#5876,#5877,#5878),
 .UNSPECIFIED.,.F.,.F.,(4,2,2,2,2,2,2,4),(-0.45424830909043,-0.396054469342604,
-0.339406675181722,-0.276261577769454,-0.221379042231552,-0.165164477779452,
-0.098609088443841,0.),.UNSPECIFIED.);
#197=B_SPLINE_CURVE_WITH_KNOTS('',3,(#5888,#5889,#5890,#5891,#5892,#5893,
#5894,#5895,#5896,#5897,#5898,#5899,#5900,#5901,#5902,#5903),
 .UNSPECIFIED.,.F.,.F.,(4,2,2,2,2,2,2,4),(-0.454158667319319,-0.395672852804858,
-0.338529950359415,-0.275786564377704,-0.221062756831308,-0.164836364834591,
-0.0983527839094977,0.),.UNSPECIFIED.);
#198=B_SPLINE_CURVE_WITH_KNOTS('',3,(#5907,#5908,#5909,#5910,#5911,#5912,
#5913,#5914,#5915,#5916,#5917,#5918,#5919,#5920,#5921,#5922),
 .UNSPECIFIED.,.F.,.F.,(4,2,2,2,2,2,2,4),(-0.46406483796248,-0.409466852189161,
-0.354565796864805,-0.295225270188452,-0.239612954364848,-0.179833767169889,
-0.105641391458423,0.),.UNSPECIFIED.);
#199=B_SPLINE_CURVE_WITH_KNOTS('',3,(#5930,#5931,#5932,#5933,#5934,#5935,
#5936,#5937),.UNSPECIFIED.,.F.,.F.,(4,2,2,4),(-0.454179041892498,-0.395759356749834,
-0.338728191012573,-0.307335875219019),.UNSPECIFIED.);
#200=B_SPLINE_CURVE_WITH_KNOTS('',3,(#5941,#5942,#5943,#5944,#5945,#5946,
#5947,#5948,#5949,#5950,#5951,#5952,#5953,#5954,#5955,#5956),
 .UNSPECIFIED.,.F.,.F.,(4,2,2,2,2,2,2,4),(-0.464072133285143,-0.40946346297479,
-0.354653577959605,-0.295254131517927,-0.239649525441963,-0.179869516594418,
-0.105654793183184,0.),.UNSPECIFIED.);
#201=B_SPLINE_CURVE_WITH_KNOTS('',3,(#5959,#5960,#5961,#5962,#5963,#5964,
#5965,#5966,#5967,#5968,#5969,#5970),.UNSPECIFIED.,.F.,.F.,(4,2,2,2,2,4),
(-0.307335875219019,-0.275894647345887,-0.221135020913433,-0.16491140803405,
-0.0984111283989864,0.),.UNSPECIFIED.);
#202=B_SPLINE_CURVE_WITH_KNOTS('',3,(#5977,#5978,#5979,#5980,#5981,#5982,
#5983,#5984,#5985,#5986,#5987,#5988,#5989,#5990,#5991,#5992),
 .UNSPECIFIED.,.F.,.F.,(4,2,2,2,2,2,2,4),(-0.454248309090363,-0.396054469342546,
-0.339406675181674,-0.276261577769416,-0.221379042231522,-0.16516447777943,
-0.0986090884438293,-0.028880024024463),.UNSPECIFIED.);
#203=B_SPLINE_CURVE_WITH_KNOTS('',3,(#5996,#5997,#5998,#5999,#6000,#6001,
#6002,#6003,#6004,#6005,#6006,#6007,#6008,#6009,#6010,#6011),
 .UNSPECIFIED.,.F.,.F.,(4,2,2,2,2,2,2,4),(-0.464097123056143,-0.409448749758071,
-0.354953921831454,-0.29535189116423,-0.239773021090806,-0.179990573569076,
-0.10570083678154,0.),.UNSPECIFIED.);
#204=B_SPLINE_CURVE_WITH_KNOTS('',3,(#6014,#6015,#6016,#6017),
 .UNSPECIFIED.,.F.,.F.,(4,4),(-0.028880024024463,0.),.UNSPECIFIED.);
#205=B_SPLINE_CURVE_WITH_KNOTS('',3,(#6024,#6025,#6026,#6027,#6028,#6029,
#6030,#6031,#6032,#6033,#6034,#6035),.UNSPECIFIED.,.F.,.F.,(4,2,2,2,2,4),
(-0.45417904189259,-0.395759356749914,-0.338728191012644,-0.275894647345943,
-0.221135020913473,-0.178087805736112),.UNSPECIFIED.);
#206=B_SPLINE_CURVE_WITH_KNOTS('',3,(#6039,#6040,#6041,#6042,#6043,#6044,
#6045,#6046,#6047,#6048,#6049,#6050,#6051,#6052,#6053,#6054),
 .UNSPECIFIED.,.F.,.F.,(4,2,2,2,2,2,2,4),(-0.464072133285183,-0.409463462974824,
-0.35465357795963,-0.295254131517949,-0.239649525441983,-0.179869516594434,
-0.10565479318319,0.),.UNSPECIFIED.);
#207=B_SPLINE_CURVE_WITH_KNOTS('',3,(#6057,#6058,#6059,#6060,#6061,#6062,
#6063,#6064),.UNSPECIFIED.,.F.,.F.,(4,2,2,4),(-0.178087805736112,-0.164911408034076,
-0.098411128398999,0.),.UNSPECIFIED.);
#208=B_SPLINE_CURVE_WITH_KNOTS('',3,(#6073,#6074,#6075,#6076,#6077,#6078,
#6079,#6080,#6081,#6082,#6083,#6084,#6085,#6086,#6087,#6088),
 .UNSPECIFIED.,.F.,.F.,(4,2,2,2,2,2,2,4),(-0.464097123055936,-0.409448749757892,
-0.354953921831303,-0.295351891164108,-0.239773021090708,-0.179990573569004,
-0.105700836781506,0.),.UNSPECIFIED.);
#209=B_SPLINE_CURVE_WITH_KNOTS('',3,(#6092,#6093,#6094,#6095,#6096,#6097,
#6098,#6099,#6100,#6101,#6102,#6103,#6104,#6105,#6106,#6107),
 .UNSPECIFIED.,.F.,.F.,(4,2,2,2,2,2,2,4),(-0.454248309090378,-0.396054469342558,
-0.339406675181681,-0.276261577769421,-0.221379042231525,-0.165164477779432,
-0.0986090884438326,0.),.UNSPECIFIED.);
#210=B_SPLINE_CURVE_WITH_KNOTS('',3,(#6117,#6118,#6119,#6120,#6121,#6122,
#6123,#6124,#6125,#6126,#6127,#6128,#6129,#6130,#6131,#6132),
 .UNSPECIFIED.,.F.,.F.,(4,2,2,2,2,2,2,4),(-0.464064837962455,-0.409466852189138,
-0.354565796864784,-0.295225270188435,-0.239612954364835,-0.17983376716988,
-0.105641391458419,0.),.UNSPECIFIED.);
#211=B_SPLINE_CURVE_WITH_KNOTS('',3,(#6136,#6137,#6138,#6139,#6140,#6141,
#6142,#6143,#6144,#6145,#6146,#6147,#6148,#6149,#6150,#6151),
 .UNSPECIFIED.,.F.,.F.,(4,2,2,2,2,2,2,4),(-0.454158667319288,-0.395672852804831,
-0.338529950359391,-0.275786564377685,-0.221062756831291,-0.164836364834576,
-0.0983527839094893,0.),.UNSPECIFIED.);
#212=B_SPLINE_CURVE_WITH_KNOTS('',3,(#6159,#6160,#6161,#6162,#6163,#6164,
#6165,#6166,#6167,#6168,#6169,#6170,#6171,#6172),.UNSPECIFIED.,.F.,.F.,
(4,2,2,2,2,2,4),(-0.464072133285276,-0.409463462974907,-0.354653577959703,
-0.295254131518009,-0.239649525442028,-0.179869516594465,-0.153354495923179),
 .UNSPECIFIED.);
#213=B_SPLINE_CURVE_WITH_KNOTS('',3,(#6176,#6177,#6178,#6179,#6180,#6181,
#6182,#6183,#6184,#6185,#6186,#6187,#6188,#6189,#6190,#6191),
 .UNSPECIFIED.,.F.,.F.,(4,2,2,2,2,2,2,4),(-0.454179041892453,-0.395759356749796,
-0.338728191012541,-0.275894647345861,-0.221135020913411,-0.164911408034033,
-0.0984111283989789,0.),.UNSPECIFIED.);
#214=B_SPLINE_CURVE_WITH_KNOTS('',3,(#6194,#6195,#6196,#6197,#6198,#6199),
 .UNSPECIFIED.,.F.,.F.,(4,2,4),(-0.153354495923179,-0.105654793183204,0.),
 .UNSPECIFIED.);
#215=B_SPLINE_CURVE_WITH_KNOTS('',3,(#6206,#6207,#6208,#6209),
 .UNSPECIFIED.,.F.,.F.,(4,4),(-0.464097123055962,-0.436632642152651),
 .UNSPECIFIED.);
#216=B_SPLINE_CURVE_WITH_KNOTS('',3,(#6213,#6214,#6215,#6216,#6217,#6218,
#6219,#6220,#6221,#6222,#6223,#6224,#6225,#6226,#6227,#6228),
 .UNSPECIFIED.,.F.,.F.,(4,2,2,2,2,2,2,4),(-0.45424830909032,-0.396054469342508,
-0.33940667518164,-0.27626157776939,-0.221379042231501,-0.165164477779415,
-0.0986090884438244,0.),.UNSPECIFIED.);
#217=B_SPLINE_CURVE_WITH_KNOTS('',3,(#6231,#6232,#6233,#6234,#6235,#6236,
#6237,#6238,#6239,#6240,#6241,#6242,#6243,#6244,#6245,#6246),
 .UNSPECIFIED.,.F.,.F.,(4,2,2,2,2,2,2,4),(-0.436632642152651,-0.409448749757915,
-0.354953921831322,-0.295351891164124,-0.239773021090723,-0.179990573569017,
-0.105700836781513,0.),.UNSPECIFIED.);
#218=B_SPLINE_CURVE_WITH_KNOTS('',3,(#6296,#6297,#6298,#6299,#6300,#6301,
#6302,#6303,#6304,#6305,#6306,#6307,#6308,#6309,#6310,#6311),
 .UNSPECIFIED.,.F.,.F.,(4,2,2,2,2,2,2,4),(-0.464072133285216,-0.409463462974853,
-0.354653577959658,-0.295254131517975,-0.239649525442001,-0.179869516594444,
-0.105654793183195,0.),.UNSPECIFIED.);
#219=B_SPLINE_CURVE_WITH_KNOTS('',3,(#6315,#6316,#6317,#6318,#6319,#6320,
#6321,#6322),.UNSPECIFIED.,.F.,.F.,(4,2,2,4),(-0.178087805736112,-0.164911408034075,
-0.098411128398998,0.),.UNSPECIFIED.);
#220=B_SPLINE_CURVE_WITH_KNOTS('',3,(#6327,#6328,#6329,#6330,#6331,#6332,
#6333,#6334,#6335,#6336,#6337,#6338),.UNSPECIFIED.,.F.,.F.,(4,2,2,2,2,4),
(-0.454179041892585,-0.395759356749908,-0.338728191012637,-0.275894647345938,
-0.221135020913471,-0.178087805736112),.UNSPECIFIED.);
#221=B_SPLINE_CURVE_WITH_KNOTS('',3,(#6343,#6344,#6345,#6346,#6347,#6348,
#6349,#6350,#6351,#6352,#6353,#6354,#6355,#6356,#6357,#6358),
 .UNSPECIFIED.,.F.,.F.,(4,2,2,2,2,2,2,4),(-0.464097123055979,-0.409448749757929,
-0.354953921831334,-0.295351891164134,-0.23977302109073,-0.179990573569022,
-0.105700836781514,0.),.UNSPECIFIED.);
#222=B_SPLINE_CURVE_WITH_KNOTS('',3,(#6362,#6363,#6364,#6365,#6366,#6367,
#6368,#6369,#6370,#6371,#6372,#6373,#6374,#6375,#6376,#6377),
 .UNSPECIFIED.,.F.,.F.,(4,2,2,2,2,2,2,4),(-0.454248309090339,-0.396054469342525,
-0.339406675181652,-0.276261577769397,-0.221379042231507,-0.16516447777942,
-0.0986090884438264,0.),.UNSPECIFIED.);
#223=B_SPLINE_CURVE_WITH_KNOTS('',3,(#6387,#6388,#6389,#6390,#6391,#6392,
#6393,#6394,#6395,#6396,#6397,#6398,#6399,#6400,#6401,#6402),
 .UNSPECIFIED.,.F.,.F.,(4,2,2,2,2,2,2,4),(-0.464064837962443,-0.40946685218913,
-0.354565796864779,-0.295225270188433,-0.239612954364833,-0.179833767169879,
-0.10564139145842,0.),.UNSPECIFIED.);
#224=B_SPLINE_CURVE_WITH_KNOTS('',3,(#6411,#6412,#6413,#6414,#6415,#6416,
#6417,#6418,#6419,#6420,#6421,#6422,#6423,#6424,#6425,#6426),
 .UNSPECIFIED.,.F.,.F.,(4,2,2,2,2,2,2,4),(-0.454158667319305,-0.395672852804848,
-0.338529950359406,-0.275786564377698,-0.221062756831303,-0.164836364834586,
-0.0983527839094943,0.),.UNSPECIFIED.);
#225=B_SPLINE_CURVE_WITH_KNOTS('',3,(#6431,#6432,#6433,#6434,#6435,#6436,
#6437,#6438,#6439,#6440,#6441,#6442,#6443,#6444),.UNSPECIFIED.,.F.,.F.,
(4,2,2,2,2,2,4),(-0.46407213328519,-0.409463462974826,-0.35465357795963,
-0.295254131517947,-0.239649525441978,-0.179869516594429,-0.153354495923151),
 .UNSPECIFIED.);
#226=B_SPLINE_CURVE_WITH_KNOTS('',3,(#6448,#6449,#6450,#6451,#6452,#6453,
#6454,#6455,#6456,#6457,#6458,#6459,#6460,#6461,#6462,#6463),
 .UNSPECIFIED.,.F.,.F.,(4,2,2,2,2,2,2,4),(-0.45417904189259,-0.395759356749915,
-0.338728191012647,-0.275894647345947,-0.221135020913479,-0.164911408034082,
-0.0984111283990018,0.),.UNSPECIFIED.);
#227=B_SPLINE_CURVE_WITH_KNOTS('',3,(#6466,#6467,#6468,#6469,#6470,#6471),
 .UNSPECIFIED.,.F.,.F.,(4,2,4),(-0.153354495923151,-0.105654793183189,0.),
 .UNSPECIFIED.);
#228=B_SPLINE_CURVE_WITH_KNOTS('',3,(#6478,#6479,#6480,#6481),
 .UNSPECIFIED.,.F.,.F.,(4,4),(-0.464097123055929,-0.436632642152621),
 .UNSPECIFIED.);
#229=B_SPLINE_CURVE_WITH_KNOTS('',3,(#6485,#6486,#6487,#6488,#6489,#6490,
#6491,#6492,#6493,#6494,#6495,#6496,#6497,#6498,#6499,#6500),
 .UNSPECIFIED.,.F.,.F.,(4,2,2,2,2,2,2,4),(-0.454248309090296,-0.396054469342484,
-0.339406675181621,-0.276261577769375,-0.221379042231491,-0.165164477779409,
-0.0986090884438205,0.),.UNSPECIFIED.);
#230=B_SPLINE_CURVE_WITH_KNOTS('',3,(#6503,#6504,#6505,#6506,#6507,#6508,
#6509,#6510,#6511,#6512,#6513,#6514,#6515,#6516,#6517,#6518),
 .UNSPECIFIED.,.F.,.F.,(4,2,2,2,2,2,2,4),(-0.436632642152621,-0.409448749757886,
-0.354953921831299,-0.295351891164106,-0.239773021090707,-0.179990573569004,
-0.105700836781506,0.),.UNSPECIFIED.);
#231=B_SPLINE_CURVE_WITH_KNOTS('',3,(#6525,#6526,#6527,#6528,#6529,#6530,
#6531,#6532,#6533,#6534),.UNSPECIFIED.,.F.,.F.,(4,2,2,2,4),(-0.46407213328521,
-0.40946346297485,-0.354653577959657,-0.295254131517975,-0.285596349669175),
 .UNSPECIFIED.);
#232=B_SPLINE_CURVE_WITH_KNOTS('',3,(#6538,#6539,#6540,#6541,#6542,#6543,
#6544,#6545,#6546,#6547,#6548,#6549,#6550,#6551,#6552,#6553),
 .UNSPECIFIED.,.F.,.F.,(4,2,2,2,2,2,2,4),(-0.454179041892491,-0.395759356749834,
-0.338728191012574,-0.275894647345886,-0.221135020913429,-0.164911408034045,
-0.0984111283989847,0.),.UNSPECIFIED.);
#233=B_SPLINE_CURVE_WITH_KNOTS('',3,(#6556,#6557,#6558,#6559,#6560,#6561,
#6562,#6563,#6564,#6565),.UNSPECIFIED.,.F.,.F.,(4,2,2,2,4),(-0.285596349669175,
-0.239649525442001,-0.179869516594444,-0.105654793183195,0.),
 .UNSPECIFIED.);
#234=B_SPLINE_CURVE_WITH_KNOTS('',3,(#6572,#6573,#6574,#6575,#6576,#6577,
#6578,#6579,#6580,#6581,#6582,#6583,#6584,#6585,#6586,#6587),
 .UNSPECIFIED.,.F.,.F.,(4,2,2,2,2,2,2,4),(-0.464097123056155,-0.409448749758082,
-0.354953921831466,-0.295351891164244,-0.239773021090817,-0.179990573569081,
-0.10570083678154,0.),.UNSPECIFIED.);
#235=B_SPLINE_CURVE_WITH_KNOTS('',3,(#6591,#6592,#6593,#6594,#6595,#6596,
#6597,#6598,#6599,#6600,#6601,#6602,#6603,#6604,#6605,#6606),
 .UNSPECIFIED.,.F.,.F.,(4,2,2,2,2,2,2,4),(-0.454248309090326,-0.396054469342517,
-0.339406675181648,-0.276261577769394,-0.221379042231504,-0.165164477779418,
-0.0986090884438254,0.),.UNSPECIFIED.);
#236=B_SPLINE_CURVE_WITH_KNOTS('',3,(#6616,#6617,#6618,#6619,#6620,#6621,
#6622,#6623,#6624,#6625,#6626,#6627,#6628,#6629,#6630,#6631),
 .UNSPECIFIED.,.F.,.F.,(4,2,2,2,2,2,2,4),(-0.464064837962487,-0.409466852189169,
-0.35456579686481,-0.295225270188456,-0.23961295436485,-0.17983376716989,
-0.105641391458424,0.),.UNSPECIFIED.);
#237=B_SPLINE_CURVE_WITH_KNOTS('',3,(#6635,#6636,#6637,#6638,#6639,#6640,
#6641,#6642,#6643,#6644,#6645,#6646,#6647,#6648,#6649,#6650),
 .UNSPECIFIED.,.F.,.F.,(4,2,2,2,2,2,2,4),(-0.454158667319304,-0.395672852804846,
-0.338529950359405,-0.275786564377698,-0.221062756831303,-0.164836364834585,
-0.0983527839094934,0.),.UNSPECIFIED.);
#238=B_SPLINE_CURVE_WITH_KNOTS('',3,(#6660,#6661,#6662,#6663,#6664,#6665,
#6666,#6667,#6668,#6669,#6670,#6671,#6672,#6673,#6674,#6675),
 .UNSPECIFIED.,.F.,.F.,(4,2,2,2,2,2,2,4),(-0.464072133285175,-0.409463462974818,
-0.354653577959626,-0.295254131517947,-0.23964952544198,-0.179869516594429,
-0.105654793183188,0.),.UNSPECIFIED.);
#239=B_SPLINE_CURVE_WITH_KNOTS('',3,(#6679,#6680,#6681,#6682,#6683,#6684,
#6685,#6686,#6687,#6688,#6689,#6690),.UNSPECIFIED.,.F.,.F.,(4,2,2,2,2,4),
(-0.307335875219043,-0.275894647345908,-0.221135020913448,-0.164911408034059,
-0.0984111283989903,0.),.UNSPECIFIED.);
#240=B_SPLINE_CURVE_WITH_KNOTS('',3,(#6695,#6696,#6697,#6698,#6699,#6700,
#6701,#6702),.UNSPECIFIED.,.F.,.F.,(4,2,2,4),(-0.454179041892519,-0.395759356749857,
-0.338728191012597,-0.307335875219043),.UNSPECIFIED.);
#241=B_SPLINE_CURVE_WITH_KNOTS('',3,(#6707,#6708,#6709,#6710,#6711,#6712,
#6713,#6714,#6715,#6716,#6717,#6718,#6719,#6720,#6721,#6722),
 .UNSPECIFIED.,.F.,.F.,(4,2,2,2,2,2,2,4),(-0.464097123055928,-0.409448749757884,
-0.354953921831297,-0.295351891164106,-0.239773021090708,-0.179990573569004,
-0.105700836781506,0.),.UNSPECIFIED.);
#242=B_SPLINE_CURVE_WITH_KNOTS('',3,(#6726,#6727,#6728,#6729),
 .UNSPECIFIED.,.F.,.F.,(4,4),(-0.028880024024466,0.),.UNSPECIFIED.);
#243=B_SPLINE_CURVE_WITH_KNOTS('',3,(#6734,#6735,#6736,#6737,#6738,#6739,
#6740,#6741,#6742,#6743,#6744,#6745,#6746,#6747,#6748,#6749),
 .UNSPECIFIED.,.F.,.F.,(4,2,2,2,2,2,2,4),(-0.454248309090515,-0.396054469342676,
-0.339406675181783,-0.276261577769502,-0.221379042231587,-0.165164477779474,
-0.0986090884438518,-0.028880024024466),.UNSPECIFIED.);
#244=B_SPLINE_CURVE_WITH_KNOTS('',3,(#7318,#7319,#7320,#7321,#7322,#7323,
#7324,#7325,#7326,#7327,#7328,#7329,#7330,#7331,#7332,#7333,#7334,#7335,
#7336,#7337,#7338,#7339),.UNSPECIFIED.,.F.,.F.,(4,2,2,2,2,2,2,2,2,2,4),
(0.0591825211272536,0.157966726598481,0.236950089897721,0.315933453196962,
0.391576304923761,0.46721915665056,0.54286200837736,0.618504860104159,0.697488223403399,
0.77647158670264,0.875255792173867),.UNSPECIFIED.);
#245=B_SPLINE_CURVE_WITH_KNOTS('',3,(#7343,#7344,#7345,#7346,#7347,#7348,
#7349,#7350,#7351,#7352,#7353,#7354,#7355,#7356,#7357,#7358,#7359,#7360,
#7361,#7362,#7363,#7364),.UNSPECIFIED.,.F.,.F.,(4,2,2,2,2,2,2,2,2,2,4),
(0.0581119756758434,0.106553146291161,0.213106292582322,0.30849933801665,
0.386091982889075,0.4636846277615,0.541277272633925,0.61886991750635,0.714262962940678,
0.820816109231839,0.869257279847157),.UNSPECIFIED.);
#246=B_SPLINE_CURVE_WITH_KNOTS('',3,(#7370,#7371,#7372,#7373,#7374,#7375,
#7376,#7377,#7378,#7379,#7380,#7381,#7382,#7383,#7384,#7385,#7386,#7387,
#7388,#7389,#7390,#7391),.UNSPECIFIED.,.F.,.F.,(4,2,2,2,2,2,2,2,2,2,4),
(0.0581119756758434,0.106553146291161,0.213106292582322,0.30849933801665,
0.386091982889075,0.4636846277615,0.541277272633925,0.61886991750635,0.714262962940679,
0.820816109231839,0.869257279847157),.UNSPECIFIED.);
#247=B_SPLINE_CURVE_WITH_KNOTS('',3,(#7395,#7396,#7397,#7398,#7399,#7400,
#7401,#7402,#7403,#7404,#7405,#7406,#7407,#7408,#7409,#7410,#7411,#7412,
#7413,#7414,#7415,#7416),.UNSPECIFIED.,.F.,.F.,(4,2,2,2,2,2,2,2,2,2,4),
(0.0581119756758433,0.106553146291161,0.213106292582322,0.308499338016649,
0.386091982889075,0.4636846277615,0.541277272633925,0.61886991750635,0.714262962940678,
0.820816109231839,0.869257279847157),.UNSPECIFIED.);
#248=B_SPLINE_CURVE_WITH_KNOTS('',3,(#7425,#7426,#7427,#7428,#7429,#7430,
#7431,#7432,#7433,#7434,#7435,#7436,#7437,#7438,#7439,#7440,#7441,#7442,
#7443,#7444,#7445,#7446),.UNSPECIFIED.,.F.,.F.,(4,2,2,2,2,2,2,2,2,2,4),
(0.0581119756758433,0.106553146291161,0.213106292582322,0.30849933801665,
0.386091982889075,0.4636846277615,0.541277272633925,0.61886991750635,0.714262962940678,
0.820816109231839,0.869257279847157),.UNSPECIFIED.);
#249=B_SPLINE_CURVE_WITH_KNOTS('',3,(#7450,#7451,#7452,#7453,#7454,#7455,
#7456,#7457,#7458,#7459,#7460,#7461,#7462,#7463,#7464,#7465,#7466,#7467,
#7468,#7469,#7470,#7471),.UNSPECIFIED.,.F.,.F.,(4,2,2,2,2,2,2,2,2,2,4),
(0.0581119756758434,0.106553146291161,0.213106292582322,0.30849933801665,
0.386091982889075,0.4636846277615,0.541277272633925,0.61886991750635,0.714262962940678,
0.820816109231839,0.869257279847157),.UNSPECIFIED.);
#250=B_SPLINE_CURVE_WITH_KNOTS('',3,(#7475,#7476,#7477,#7478,#7479,#7480,
#7481,#7482,#7483,#7484,#7485,#7486,#7487,#7488,#7489,#7490,#7491,#7492,
#7493,#7494,#7495,#7496),.UNSPECIFIED.,.F.,.F.,(4,2,2,2,2,2,2,2,2,2,4),
(0.0581119756758434,0.106553146291161,0.213106292582322,0.30849933801665,
0.386091982889075,0.4636846277615,0.541277272633925,0.61886991750635,0.714262962940678,
0.820816109231839,0.869257279847157),.UNSPECIFIED.);
#251=B_SPLINE_CURVE_WITH_KNOTS('',3,(#7500,#7501,#7502,#7503,#7504,#7505,
#7506,#7507,#7508,#7509,#7510,#7511,#7512,#7513,#7514,#7515,#7516,#7517,
#7518,#7519,#7520,#7521),.UNSPECIFIED.,.F.,.F.,(4,2,2,2,2,2,2,2,2,2,4),
(0.0581119756758433,0.106553146291161,0.213106292582322,0.30849933801665,
0.386091982889075,0.4636846277615,0.541277272633925,0.61886991750635,0.714262962940678,
0.820816109231839,0.869257279847157),.UNSPECIFIED.);
#252=B_SPLINE_CURVE_WITH_KNOTS('',3,(#7529,#7530,#7531,#7532,#7533,#7534,
#7535,#7536,#7537,#7538,#7539,#7540,#7541,#7542,#7543,#7544,#7545,#7546,
#7547,#7548,#7549,#7550),.UNSPECIFIED.,.F.,.F.,(4,2,2,2,2,2,2,2,2,2,4),
(0.0591825211272536,0.157966726598481,0.236950089897721,0.315933453196962,
0.391576304923761,0.467219156650561,0.54286200837736,0.618504860104159,
0.697488223403399,0.77647158670264,0.875255792173867),.UNSPECIFIED.);
#253=B_SPLINE_CURVE_WITH_KNOTS('',3,(#7558,#7559,#7560,#7561,#7562,#7563,
#7564,#7565,#7566,#7567,#7568,#7569,#7570,#7571,#7572,#7573,#7574,#7575,
#7576,#7577,#7578,#7579),.UNSPECIFIED.,.F.,.F.,(4,2,2,2,2,2,2,2,2,2,4),
(0.0591825211272536,0.157966726598481,0.236950089897722,0.315933453196962,
0.391576304923761,0.467219156650561,0.54286200837736,0.618504860104159,
0.697488223403399,0.77647158670264,0.875255792173867),.UNSPECIFIED.);
#254=B_SPLINE_CURVE_WITH_KNOTS('',3,(#7589,#7590,#7591,#7592,#7593,#7594,
#7595,#7596,#7597,#7598,#7599,#7600,#7601,#7602,#7603,#7604,#7605,#7606,
#7607,#7608,#7609,#7610),.UNSPECIFIED.,.F.,.F.,(4,2,2,2,2,2,2,2,2,2,4),
(0.0591825211272536,0.157966726598481,0.236950089897721,0.315933453196962,
0.391576304923761,0.46721915665056,0.54286200837736,0.618504860104159,0.697488223403399,
0.77647158670264,0.875255792173867),.UNSPECIFIED.);
#255=B_SPLINE_CURVE_WITH_KNOTS('',3,(#7618,#7619,#7620,#7621,#7622,#7623,
#7624,#7625,#7626,#7627,#7628,#7629,#7630,#7631,#7632,#7633,#7634,#7635,
#7636,#7637,#7638,#7639),.UNSPECIFIED.,.F.,.F.,(4,2,2,2,2,2,2,2,2,2,4),
(0.0591825211272536,0.157966726598481,0.236950089897721,0.315933453196962,
0.391576304923761,0.46721915665056,0.542862008377359,0.618504860104159,
0.697488223403399,0.776471586702639,0.875255792173867),.UNSPECIFIED.);
#256=B_SPLINE_CURVE_WITH_KNOTS('',3,(#7647,#7648,#7649,#7650,#7651,#7652,
#7653,#7654,#7655,#7656,#7657,#7658,#7659,#7660,#7661,#7662,#7663,#7664,
#7665,#7666,#7667,#7668),.UNSPECIFIED.,.F.,.F.,(4,2,2,2,2,2,2,2,2,2,4),
(0.0591825211272536,0.157966726598481,0.236950089897721,0.315933453196962,
0.391576304923761,0.46721915665056,0.54286200837736,0.618504860104159,0.697488223403399,
0.77647158670264,0.875255792173867),.UNSPECIFIED.);
#257=B_SPLINE_CURVE_WITH_KNOTS('',3,(#7677,#7678,#7679,#7680,#7681,#7682,
#7683,#7684,#7685,#7686,#7687,#7688,#7689,#7690,#7691,#7692,#7693,#7694,
#7695,#7696,#7697,#7698),.UNSPECIFIED.,.F.,.F.,(4,2,2,2,2,2,2,2,2,2,4),
(0.0591825211272536,0.157966726598481,0.236950089897721,0.315933453196962,
0.391576304923761,0.46721915665056,0.542862008377359,0.618504860104159,
0.697488223403399,0.776471586702639,0.875255792173867),.UNSPECIFIED.);
#258=SHAPE_REPRESENTATION_RELATIONSHIP('SRR','None',#7903,#278);
#259=SHAPE_REPRESENTATION_RELATIONSHIP('SRR','None',#7904,#279);
#260=SHAPE_REPRESENTATION_RELATIONSHIP('SRR','None',#7906,#280);
#261=SHAPE_REPRESENTATION_RELATIONSHIP('SRR','None',#7907,#281);
#262=SHAPE_REPRESENTATION_RELATIONSHIP('SRR','None',#7908,#282);
#263=SHAPE_REPRESENTATION_RELATIONSHIP('SRR','None',#7909,#283);
#264=SHAPE_REPRESENTATION_RELATIONSHIP('SRR','None',#7910,#284);
#265=SHAPE_REPRESENTATION_RELATIONSHIP('SRR','None',#7912,#285);
#266=SHAPE_REPRESENTATION_RELATIONSHIP('SRR','None',#7913,#286);
#267=SHAPE_REPRESENTATION_RELATIONSHIP('SRR','None',#7914,#287);
#268=SHAPE_REPRESENTATION_RELATIONSHIP('SRR','None',#7915,#288);
#269=SHAPE_REPRESENTATION_RELATIONSHIP('SRR','None',#7916,#289);
#270=SHAPE_REPRESENTATION_RELATIONSHIP('SRR','None',#7917,#290);
#271=SHAPE_REPRESENTATION_RELATIONSHIP('SRR','None',#7919,#291);
#272=SHAPE_REPRESENTATION_RELATIONSHIP('SRR','None',#7921,#292);
#273=SHAPE_REPRESENTATION_RELATIONSHIP('SRR','None',#7922,#293);
#274=SHAPE_REPRESENTATION_RELATIONSHIP('SRR','None',#7923,#294);
#275=SHAPE_REPRESENTATION_RELATIONSHIP('SRR','None',#7924,#295);
#276=SHAPE_REPRESENTATION_RELATIONSHIP('SRR','None',#7925,#296);
#277=SHAPE_REPRESENTATION_RELATIONSHIP('SRR','None',#7926,#297);
#278=ADVANCED_BREP_SHAPE_REPRESENTATION('',(#334),#7792);
#279=ADVANCED_BREP_SHAPE_REPRESENTATION('',(#335),#7793);
#280=ADVANCED_BREP_SHAPE_REPRESENTATION('',(#336),#7795);
#281=ADVANCED_BREP_SHAPE_REPRESENTATION('',(#337),#7796);
#282=ADVANCED_BREP_SHAPE_REPRESENTATION('',(#338,#339,#340,#341,#342,#343,
#344,#345,#346,#347),#7797);
#283=ADVANCED_BREP_SHAPE_REPRESENTATION('',(#348),#7798);
#284=ADVANCED_BREP_SHAPE_REPRESENTATION('',(#349),#7799);
#285=ADVANCED_BREP_SHAPE_REPRESENTATION('',(#350),#7801);
#286=ADVANCED_BREP_SHAPE_REPRESENTATION('',(#351),#7802);
#287=ADVANCED_BREP_SHAPE_REPRESENTATION('',(#352),#7803);
#288=ADVANCED_BREP_SHAPE_REPRESENTATION('',(#353),#7804);
#289=ADVANCED_BREP_SHAPE_REPRESENTATION('',(#354),#7805);
#290=ADVANCED_BREP_SHAPE_REPRESENTATION('',(#12),#7806);
#291=ADVANCED_BREP_SHAPE_REPRESENTATION('',(#355),#7808);
#292=ADVANCED_BREP_SHAPE_REPRESENTATION('',(#356),#7810);
#293=ADVANCED_BREP_SHAPE_REPRESENTATION('',(#357),#7811);
#294=ADVANCED_BREP_SHAPE_REPRESENTATION('',(#358,#359,#360,#361,#362,#363,
#364),#7812);
#295=ADVANCED_BREP_SHAPE_REPRESENTATION('',(#365),#7813);
#296=ADVANCED_BREP_SHAPE_REPRESENTATION('',(#366,#367),#7814);
#297=ADVANCED_BREP_SHAPE_REPRESENTATION('',(#368),#7815);
#298=STYLED_ITEM('',(#8111),#334);
#299=STYLED_ITEM('',(#8097),#335);
#300=STYLED_ITEM('',(#8104),#336);
#301=STYLED_ITEM('',(#8104),#337);
#302=STYLED_ITEM('',(#8097),#338);
#303=STYLED_ITEM('',(#8097),#339);
#304=STYLED_ITEM('',(#8097),#340);
#305=STYLED_ITEM('',(#8097),#341);
#306=STYLED_ITEM('',(#8097),#342);
#307=STYLED_ITEM('',(#8097),#343);
#308=STYLED_ITEM('',(#8097),#344);
#309=STYLED_ITEM('',(#8097),#345);
#310=STYLED_ITEM('',(#8097),#346);
#311=STYLED_ITEM('',(#8097),#347);
#312=STYLED_ITEM('',(#8104),#348);
#313=STYLED_ITEM('',(#8104),#349);
#314=STYLED_ITEM('',(#8097),#350);
#315=STYLED_ITEM('',(#8090),#351);
#316=STYLED_ITEM('',(#8097),#352);
#317=STYLED_ITEM('',(#8097),#353);
#318=STYLED_ITEM('',(#8097),#354);
#319=STYLED_ITEM('',(#8104),#12);
#320=STYLED_ITEM('',(#8097),#355);
#321=STYLED_ITEM('',(#8097),#356);
#322=STYLED_ITEM('',(#8097),#357);
#323=STYLED_ITEM('',(#8097),#358);
#324=STYLED_ITEM('',(#8097),#359);
#325=STYLED_ITEM('',(#8097),#360);
#326=STYLED_ITEM('',(#8097),#361);
#327=STYLED_ITEM('',(#8097),#362);
#328=STYLED_ITEM('',(#8097),#363);
#329=STYLED_ITEM('',(#8097),#364);
#330=STYLED_ITEM('',(#8097),#365);
#331=STYLED_ITEM('',(#8097),#366);
#332=STYLED_ITEM('',(#8097),#367);
#333=STYLED_ITEM('',(#8097),#368);
#334=MANIFOLD_SOLID_BREP('Body1',#3704);
#335=MANIFOLD_SOLID_BREP('Body1',#3705);
#336=MANIFOLD_SOLID_BREP('Body1',#3706);
#337=MANIFOLD_SOLID_BREP('Body1',#3707);
#338=MANIFOLD_SOLID_BREP('Body1',#3708);
#339=MANIFOLD_SOLID_BREP('Body2',#3709);
#340=MANIFOLD_SOLID_BREP('Body3',#3710);
#341=MANIFOLD_SOLID_BREP('Body4',#3711);
#342=MANIFOLD_SOLID_BREP('Body5',#3712);
#343=MANIFOLD_SOLID_BREP('Body6',#3713);
#344=MANIFOLD_SOLID_BREP('Body7',#3714);
#345=MANIFOLD_SOLID_BREP('Body8',#3715);
#346=MANIFOLD_SOLID_BREP('Body9',#3716);
#347=MANIFOLD_SOLID_BREP('Body10',#3717);
#348=MANIFOLD_SOLID_BREP('Body1',#3718);
#349=MANIFOLD_SOLID_BREP('Body1',#3719);
#350=MANIFOLD_SOLID_BREP('Body1',#3720);
#351=MANIFOLD_SOLID_BREP('Body1',#3721);
#352=MANIFOLD_SOLID_BREP('Body1',#3722);
#353=MANIFOLD_SOLID_BREP('Body1',#3723);
#354=MANIFOLD_SOLID_BREP('Body1',#3724);
#355=MANIFOLD_SOLID_BREP('Body1',#3727);
#356=MANIFOLD_SOLID_BREP('Body1',#3728);
#357=MANIFOLD_SOLID_BREP('Body1',#3729);
#358=MANIFOLD_SOLID_BREP('Body1',#3730);
#359=MANIFOLD_SOLID_BREP('Body2',#3731);
#360=MANIFOLD_SOLID_BREP('Body3',#3732);
#361=MANIFOLD_SOLID_BREP('Body4',#3733);
#362=MANIFOLD_SOLID_BREP('Body5',#3734);
#363=MANIFOLD_SOLID_BREP('Body6',#3735);
#364=MANIFOLD_SOLID_BREP('Body7',#3736);
#365=MANIFOLD_SOLID_BREP('Continuous crown cage',#3737);
#366=MANIFOLD_SOLID_BREP('Body1',#3738);
#367=MANIFOLD_SOLID_BREP('Body2',#3739);
#368=MANIFOLD_SOLID_BREP('Body1',#3740);
#369=FACE_BOUND('',#743,.T.);
#370=FACE_BOUND('',#744,.T.);
#371=FACE_BOUND('',#745,.T.);
#372=FACE_BOUND('',#746,.T.);
#373=FACE_BOUND('',#747,.T.);
#374=FACE_BOUND('',#749,.T.);
#375=FACE_BOUND('',#750,.T.);
#376=FACE_BOUND('',#751,.T.);
#377=FACE_BOUND('',#752,.T.);
#378=FACE_BOUND('',#753,.T.);
#379=FACE_BOUND('',#757,.T.);
#380=FACE_BOUND('',#761,.T.);
#381=FACE_BOUND('',#765,.T.);
#382=FACE_BOUND('',#777,.T.);
#383=FACE_BOUND('',#789,.T.);
#384=FACE_BOUND('',#792,.T.);
#385=FACE_BOUND('',#793,.T.);
#386=FACE_BOUND('',#794,.T.);
#387=FACE_BOUND('',#795,.T.);
#388=FACE_BOUND('',#796,.T.);
#389=FACE_BOUND('',#797,.T.);
#390=FACE_BOUND('',#798,.T.);
#391=FACE_BOUND('',#799,.T.);
#392=FACE_BOUND('',#800,.T.);
#393=FACE_BOUND('',#801,.T.);
#394=FACE_BOUND('',#802,.T.);
#395=FACE_BOUND('',#815,.T.);
#396=FACE_BOUND('',#827,.T.);
#397=FACE_BOUND('',#828,.T.);
#398=FACE_BOUND('',#829,.T.);
#399=FACE_BOUND('',#830,.T.);
#400=FACE_BOUND('',#831,.T.);
#401=FACE_BOUND('',#832,.T.);
#402=FACE_BOUND('',#833,.T.);
#403=FACE_BOUND('',#834,.T.);
#404=FACE_BOUND('',#835,.T.);
#405=FACE_BOUND('',#836,.T.);
#406=FACE_BOUND('',#837,.T.);
#407=FACE_BOUND('',#840,.T.);
#408=FACE_BOUND('',#855,.T.);
#409=FACE_BOUND('',#857,.T.);
#410=FACE_BOUND('',#868,.T.);
#411=FACE_BOUND('',#870,.T.);
#412=FACE_BOUND('',#883,.T.);
#413=FACE_BOUND('',#891,.T.);
#414=FACE_BOUND('',#895,.T.);
#415=FACE_BOUND('',#897,.T.);
#416=FACE_BOUND('',#901,.T.);
#417=FACE_BOUND('',#906,.T.);
#418=FACE_BOUND('',#910,.T.);
#419=FACE_BOUND('',#912,.T.);
#420=FACE_BOUND('',#916,.T.);
#421=FACE_BOUND('',#918,.T.);
#422=FACE_BOUND('',#933,.T.);
#423=FACE_BOUND('',#938,.T.);
#424=FACE_BOUND('',#941,.T.);
#425=FACE_BOUND('',#945,.T.);
#426=FACE_BOUND('',#947,.T.);
#427=FACE_BOUND('',#953,.T.);
#428=FACE_BOUND('',#956,.T.);
#429=FACE_BOUND('',#961,.T.);
#430=FACE_BOUND('',#966,.T.);
#431=FACE_BOUND('',#991,.T.);
#432=FACE_BOUND('',#994,.T.);
#433=FACE_BOUND('',#997,.T.);
#434=FACE_BOUND('',#1000,.T.);
#435=FACE_BOUND('',#1003,.T.);
#436=FACE_BOUND('',#1008,.T.);
#437=FACE_BOUND('',#1010,.T.);
#438=PLANE('',#3980);
#439=PLANE('',#3981);
#440=PLANE('',#3982);
#441=PLANE('',#3983);
#442=PLANE('',#3984);
#443=PLANE('',#3985);
#444=PLANE('',#3990);
#445=PLANE('',#3991);
#446=PLANE('',#3996);
#447=PLANE('',#3997);
#448=PLANE('',#4003);
#449=PLANE('',#4050);
#450=PLANE('',#4082);
#451=PLANE('',#4086);
#452=PLANE('',#4134);
#453=PLANE('',#4166);
#454=PLANE('',#4171);
#455=PLANE('',#4204);
#456=PLANE('',#4205);
#457=PLANE('',#4211);
#458=PLANE('',#4212);
#459=PLANE('',#4213);
#460=PLANE('',#4217);
#461=PLANE('',#4218);
#462=PLANE('',#4219);
#463=PLANE('',#4220);
#464=PLANE('',#4221);
#465=PLANE('',#4238);
#466=PLANE('',#4239);
#467=PLANE('',#4240);
#468=PLANE('',#4241);
#469=PLANE('',#4242);
#470=PLANE('',#4243);
#471=PLANE('',#4244);
#472=PLANE('',#4245);
#473=PLANE('',#4246);
#474=PLANE('',#4247);
#475=PLANE('',#4248);
#476=PLANE('',#4249);
#477=PLANE('',#4250);
#478=PLANE('',#4251);
#479=PLANE('',#4252);
#480=PLANE('',#4253);
#481=PLANE('',#4261);
#482=PLANE('',#4262);
#483=PLANE('',#4267);
#484=PLANE('',#4268);
#485=PLANE('',#4273);
#486=PLANE('',#4276);
#487=PLANE('',#4284);
#488=PLANE('',#4285);
#489=PLANE('',#4293);
#490=PLANE('',#4294);
#491=PLANE('',#4296);
#492=PLANE('',#4297);
#493=PLANE('',#4298);
#494=PLANE('',#4299);
#495=PLANE('',#4300);
#496=PLANE('',#4301);
#497=PLANE('',#4302);
#498=PLANE('',#4303);
#499=PLANE('',#4304);
#500=PLANE('',#4306);
#501=PLANE('',#4314);
#502=PLANE('',#4331);
#503=PLANE('',#4336);
#504=PLANE('',#4342);
#505=PLANE('',#4343);
#506=PLANE('',#4359);
#507=PLANE('',#4362);
#508=PLANE('',#4374);
#509=PLANE('',#4383);
#510=PLANE('',#4414);
#511=PLANE('',#4419);
#512=PLANE('',#4424);
#513=PLANE('',#4430);
#514=PLANE('',#4435);
#515=PLANE('',#4444);
#516=PLANE('',#4448);
#517=PLANE('',#4449);
#518=PLANE('',#4451);
#519=PLANE('',#4456);
#520=PLANE('',#4459);
#521=PLANE('',#4464);
#522=PLANE('',#4479);
#523=PLANE('',#4480);
#524=FACE_OUTER_BOUND('',#733,.T.);
#525=FACE_OUTER_BOUND('',#734,.T.);
#526=FACE_OUTER_BOUND('',#735,.T.);
#527=FACE_OUTER_BOUND('',#736,.T.);
#528=FACE_OUTER_BOUND('',#737,.T.);
#529=FACE_OUTER_BOUND('',#738,.T.);
#530=FACE_OUTER_BOUND('',#739,.T.);
#531=FACE_OUTER_BOUND('',#740,.T.);
#532=FACE_OUTER_BOUND('',#741,.T.);
#533=FACE_OUTER_BOUND('',#742,.T.);
#534=FACE_OUTER_BOUND('',#748,.T.);
#535=FACE_OUTER_BOUND('',#754,.T.);
#536=FACE_OUTER_BOUND('',#755,.T.);
#537=FACE_OUTER_BOUND('',#756,.T.);
#538=FACE_OUTER_BOUND('',#758,.T.);
#539=FACE_OUTER_BOUND('',#759,.T.);
#540=FACE_OUTER_BOUND('',#760,.T.);
#541=FACE_OUTER_BOUND('',#762,.T.);
#542=FACE_OUTER_BOUND('',#763,.T.);
#543=FACE_OUTER_BOUND('',#764,.T.);
#544=FACE_OUTER_BOUND('',#766,.T.);
#545=FACE_OUTER_BOUND('',#767,.T.);
#546=FACE_OUTER_BOUND('',#768,.T.);
#547=FACE_OUTER_BOUND('',#769,.T.);
#548=FACE_OUTER_BOUND('',#770,.T.);
#549=FACE_OUTER_BOUND('',#771,.T.);
#550=FACE_OUTER_BOUND('',#772,.T.);
#551=FACE_OUTER_BOUND('',#773,.T.);
#552=FACE_OUTER_BOUND('',#774,.T.);
#553=FACE_OUTER_BOUND('',#775,.T.);
#554=FACE_OUTER_BOUND('',#776,.T.);
#555=FACE_OUTER_BOUND('',#778,.T.);
#556=FACE_OUTER_BOUND('',#779,.T.);
#557=FACE_OUTER_BOUND('',#780,.T.);
#558=FACE_OUTER_BOUND('',#781,.T.);
#559=FACE_OUTER_BOUND('',#782,.T.);
#560=FACE_OUTER_BOUND('',#783,.T.);
#561=FACE_OUTER_BOUND('',#784,.T.);
#562=FACE_OUTER_BOUND('',#785,.T.);
#563=FACE_OUTER_BOUND('',#786,.T.);
#564=FACE_OUTER_BOUND('',#787,.T.);
#565=FACE_OUTER_BOUND('',#788,.T.);
#566=FACE_OUTER_BOUND('',#790,.T.);
#567=FACE_OUTER_BOUND('',#791,.T.);
#568=FACE_OUTER_BOUND('',#803,.T.);
#569=FACE_OUTER_BOUND('',#804,.T.);
#570=FACE_OUTER_BOUND('',#805,.T.);
#571=FACE_OUTER_BOUND('',#806,.T.);
#572=FACE_OUTER_BOUND('',#807,.T.);
#573=FACE_OUTER_BOUND('',#808,.T.);
#574=FACE_OUTER_BOUND('',#809,.T.);
#575=FACE_OUTER_BOUND('',#810,.T.);
#576=FACE_OUTER_BOUND('',#811,.T.);
#577=FACE_OUTER_BOUND('',#812,.T.);
#578=FACE_OUTER_BOUND('',#813,.T.);
#579=FACE_OUTER_BOUND('',#814,.T.);
#580=FACE_OUTER_BOUND('',#816,.T.);
#581=FACE_OUTER_BOUND('',#817,.T.);
#582=FACE_OUTER_BOUND('',#818,.T.);
#583=FACE_OUTER_BOUND('',#819,.T.);
#584=FACE_OUTER_BOUND('',#820,.T.);
#585=FACE_OUTER_BOUND('',#821,.T.);
#586=FACE_OUTER_BOUND('',#822,.T.);
#587=FACE_OUTER_BOUND('',#823,.T.);
#588=FACE_OUTER_BOUND('',#824,.T.);
#589=FACE_OUTER_BOUND('',#825,.T.);
#590=FACE_OUTER_BOUND('',#826,.T.);
#591=FACE_OUTER_BOUND('',#838,.T.);
#592=FACE_OUTER_BOUND('',#839,.T.);
#593=FACE_OUTER_BOUND('',#841,.T.);
#594=FACE_OUTER_BOUND('',#842,.T.);
#595=FACE_OUTER_BOUND('',#843,.T.);
#596=FACE_OUTER_BOUND('',#844,.T.);
#597=FACE_OUTER_BOUND('',#845,.T.);
#598=FACE_OUTER_BOUND('',#846,.T.);
#599=FACE_OUTER_BOUND('',#847,.T.);
#600=FACE_OUTER_BOUND('',#848,.T.);
#601=FACE_OUTER_BOUND('',#849,.T.);
#602=FACE_OUTER_BOUND('',#850,.T.);
#603=FACE_OUTER_BOUND('',#851,.T.);
#604=FACE_OUTER_BOUND('',#852,.T.);
#605=FACE_OUTER_BOUND('',#853,.T.);
#606=FACE_OUTER_BOUND('',#854,.T.);
#607=FACE_OUTER_BOUND('',#856,.T.);
#608=FACE_OUTER_BOUND('',#858,.T.);
#609=FACE_OUTER_BOUND('',#859,.T.);
#610=FACE_OUTER_BOUND('',#860,.T.);
#611=FACE_OUTER_BOUND('',#861,.T.);
#612=FACE_OUTER_BOUND('',#862,.T.);
#613=FACE_OUTER_BOUND('',#863,.T.);
#614=FACE_OUTER_BOUND('',#864,.T.);
#615=FACE_OUTER_BOUND('',#865,.T.);
#616=FACE_OUTER_BOUND('',#866,.T.);
#617=FACE_OUTER_BOUND('',#867,.T.);
#618=FACE_OUTER_BOUND('',#869,.T.);
#619=FACE_OUTER_BOUND('',#871,.T.);
#620=FACE_OUTER_BOUND('',#872,.T.);
#621=FACE_OUTER_BOUND('',#873,.T.);
#622=FACE_OUTER_BOUND('',#874,.T.);
#623=FACE_OUTER_BOUND('',#875,.T.);
#624=FACE_OUTER_BOUND('',#876,.T.);
#625=FACE_OUTER_BOUND('',#877,.T.);
#626=FACE_OUTER_BOUND('',#878,.T.);
#627=FACE_OUTER_BOUND('',#879,.T.);
#628=FACE_OUTER_BOUND('',#880,.T.);
#629=FACE_OUTER_BOUND('',#881,.T.);
#630=FACE_OUTER_BOUND('',#882,.T.);
#631=FACE_OUTER_BOUND('',#884,.T.);
#632=FACE_OUTER_BOUND('',#885,.T.);
#633=FACE_OUTER_BOUND('',#886,.T.);
#634=FACE_OUTER_BOUND('',#887,.T.);
#635=FACE_OUTER_BOUND('',#888,.T.);
#636=FACE_OUTER_BOUND('',#889,.T.);
#637=FACE_OUTER_BOUND('',#890,.T.);
#638=FACE_OUTER_BOUND('',#892,.T.);
#639=FACE_OUTER_BOUND('',#893,.T.);
#640=FACE_OUTER_BOUND('',#894,.T.);
#641=FACE_OUTER_BOUND('',#896,.T.);
#642=FACE_OUTER_BOUND('',#898,.T.);
#643=FACE_OUTER_BOUND('',#899,.T.);
#644=FACE_OUTER_BOUND('',#900,.T.);
#645=FACE_OUTER_BOUND('',#902,.T.);
#646=FACE_OUTER_BOUND('',#903,.T.);
#647=FACE_OUTER_BOUND('',#904,.T.);
#648=FACE_OUTER_BOUND('',#905,.T.);
#649=FACE_OUTER_BOUND('',#907,.T.);
#650=FACE_OUTER_BOUND('',#908,.T.);
#651=FACE_OUTER_BOUND('',#909,.T.);
#652=FACE_OUTER_BOUND('',#911,.T.);
#653=FACE_OUTER_BOUND('',#913,.T.);
#654=FACE_OUTER_BOUND('',#914,.T.);
#655=FACE_OUTER_BOUND('',#915,.T.);
#656=FACE_OUTER_BOUND('',#917,.T.);
#657=FACE_OUTER_BOUND('',#919,.T.);
#658=FACE_OUTER_BOUND('',#920,.T.);
#659=FACE_OUTER_BOUND('',#921,.T.);
#660=FACE_OUTER_BOUND('',#922,.T.);
#661=FACE_OUTER_BOUND('',#923,.T.);
#662=FACE_OUTER_BOUND('',#924,.T.);
#663=FACE_OUTER_BOUND('',#925,.T.);
#664=FACE_OUTER_BOUND('',#926,.T.);
#665=FACE_OUTER_BOUND('',#927,.T.);
#666=FACE_OUTER_BOUND('',#928,.T.);
#667=FACE_OUTER_BOUND('',#929,.T.);
#668=FACE_OUTER_BOUND('',#930,.T.);
#669=FACE_OUTER_BOUND('',#931,.T.);
#670=FACE_OUTER_BOUND('',#932,.T.);
#671=FACE_OUTER_BOUND('',#934,.T.);
#672=FACE_OUTER_BOUND('',#935,.T.);
#673=FACE_OUTER_BOUND('',#936,.T.);
#674=FACE_OUTER_BOUND('',#937,.T.);
#675=FACE_OUTER_BOUND('',#939,.T.);
#676=FACE_OUTER_BOUND('',#940,.T.);
#677=FACE_OUTER_BOUND('',#942,.T.);
#678=FACE_OUTER_BOUND('',#943,.T.);
#679=FACE_OUTER_BOUND('',#944,.T.);
#680=FACE_OUTER_BOUND('',#946,.T.);
#681=FACE_OUTER_BOUND('',#948,.T.);
#682=FACE_OUTER_BOUND('',#949,.T.);
#683=FACE_OUTER_BOUND('',#950,.T.);
#684=FACE_OUTER_BOUND('',#951,.T.);
#685=FACE_OUTER_BOUND('',#952,.T.);
#686=FACE_OUTER_BOUND('',#954,.T.);
#687=FACE_OUTER_BOUND('',#955,.T.);
#688=FACE_OUTER_BOUND('',#957,.T.);
#689=FACE_OUTER_BOUND('',#958,.T.);
#690=FACE_OUTER_BOUND('',#959,.T.);
#691=FACE_OUTER_BOUND('',#960,.T.);
#692=FACE_OUTER_BOUND('',#962,.T.);
#693=FACE_OUTER_BOUND('',#963,.T.);
#694=FACE_OUTER_BOUND('',#964,.T.);
#695=FACE_OUTER_BOUND('',#965,.T.);
#696=FACE_OUTER_BOUND('',#967,.T.);
#697=FACE_OUTER_BOUND('',#968,.T.);
#698=FACE_OUTER_BOUND('',#969,.T.);
#699=FACE_OUTER_BOUND('',#970,.T.);
#700=FACE_OUTER_BOUND('',#971,.T.);
#701=FACE_OUTER_BOUND('',#972,.T.);
#702=FACE_OUTER_BOUND('',#973,.T.);
#703=FACE_OUTER_BOUND('',#974,.T.);
#704=FACE_OUTER_BOUND('',#975,.T.);
#705=FACE_OUTER_BOUND('',#976,.T.);
#706=FACE_OUTER_BOUND('',#977,.T.);
#707=FACE_OUTER_BOUND('',#978,.T.);
#708=FACE_OUTER_BOUND('',#979,.T.);
#709=FACE_OUTER_BOUND('',#980,.T.);
#710=FACE_OUTER_BOUND('',#981,.T.);
#711=FACE_OUTER_BOUND('',#982,.T.);
#712=FACE_OUTER_BOUND('',#983,.T.);
#713=FACE_OUTER_BOUND('',#984,.T.);
#714=FACE_OUTER_BOUND('',#985,.T.);
#715=FACE_OUTER_BOUND('',#986,.T.);
#716=FACE_OUTER_BOUND('',#987,.T.);
#717=FACE_OUTER_BOUND('',#988,.T.);
#718=FACE_OUTER_BOUND('',#989,.T.);
#719=FACE_OUTER_BOUND('',#990,.T.);
#720=FACE_OUTER_BOUND('',#992,.T.);
#721=FACE_OUTER_BOUND('',#993,.T.);
#722=FACE_OUTER_BOUND('',#995,.T.);
#723=FACE_OUTER_BOUND('',#996,.T.);
#724=FACE_OUTER_BOUND('',#998,.T.);
#725=FACE_OUTER_BOUND('',#999,.T.);
#726=FACE_OUTER_BOUND('',#1001,.T.);
#727=FACE_OUTER_BOUND('',#1002,.T.);
#728=FACE_OUTER_BOUND('',#1004,.T.);
#729=FACE_OUTER_BOUND('',#1005,.T.);
#730=FACE_OUTER_BOUND('',#1006,.T.);
#731=FACE_OUTER_BOUND('',#1007,.T.);
#732=FACE_OUTER_BOUND('',#1009,.T.);
#733=EDGE_LOOP('',(#2433,#2434,#2435,#2436));
#734=EDGE_LOOP('',(#2437,#2438,#2439,#2440));
#735=EDGE_LOOP('',(#2441,#2442,#2443,#2444));
#736=EDGE_LOOP('',(#2445,#2446,#2447,#2448));
#737=EDGE_LOOP('',(#2449,#2450,#2451,#2452));
#738=EDGE_LOOP('',(#2453,#2454,#2455,#2456));
#739=EDGE_LOOP('',(#2457,#2458,#2459,#2460));
#740=EDGE_LOOP('',(#2461,#2462,#2463,#2464));
#741=EDGE_LOOP('',(#2465,#2466,#2467,#2468));
#742=EDGE_LOOP('',(#2469,#2470,#2471,#2472));
#743=EDGE_LOOP('',(#2473));
#744=EDGE_LOOP('',(#2474));
#745=EDGE_LOOP('',(#2475));
#746=EDGE_LOOP('',(#2476));
#747=EDGE_LOOP('',(#2477));
#748=EDGE_LOOP('',(#2478,#2479,#2480,#2481));
#749=EDGE_LOOP('',(#2482));
#750=EDGE_LOOP('',(#2483));
#751=EDGE_LOOP('',(#2484));
#752=EDGE_LOOP('',(#2485));
#753=EDGE_LOOP('',(#2486));
#754=EDGE_LOOP('',(#2487,#2488,#2489,#2490));
#755=EDGE_LOOP('',(#2491));
#756=EDGE_LOOP('',(#2492));
#757=EDGE_LOOP('',(#2493));
#758=EDGE_LOOP('',(#2494,#2495,#2496,#2497));
#759=EDGE_LOOP('',(#2498));
#760=EDGE_LOOP('',(#2499));
#761=EDGE_LOOP('',(#2500));
#762=EDGE_LOOP('',(#2501,#2502,#2503,#2504));
#763=EDGE_LOOP('',(#2505,#2506,#2507,#2508));
#764=EDGE_LOOP('',(#2509));
#765=EDGE_LOOP('',(#2510));
#766=EDGE_LOOP('',(#2511,#2512,#2513,#2514,#2515,#2516,#2517,#2518));
#767=EDGE_LOOP('',(#2519,#2520,#2521,#2522,#2523,#2524,#2525,#2526));
#768=EDGE_LOOP('',(#2527,#2528,#2529,#2530,#2531,#2532,#2533,#2534));
#769=EDGE_LOOP('',(#2535,#2536,#2537,#2538,#2539,#2540,#2541,#2542));
#770=EDGE_LOOP('',(#2543,#2544,#2545,#2546,#2547,#2548,#2549,#2550));
#771=EDGE_LOOP('',(#2551,#2552,#2553,#2554,#2555,#2556,#2557,#2558));
#772=EDGE_LOOP('',(#2559,#2560,#2561,#2562,#2563,#2564,#2565,#2566));
#773=EDGE_LOOP('',(#2567,#2568,#2569,#2570,#2571,#2572,#2573,#2574));
#774=EDGE_LOOP('',(#2575,#2576,#2577,#2578,#2579,#2580,#2581,#2582));
#775=EDGE_LOOP('',(#2583,#2584,#2585,#2586,#2587,#2588,#2589,#2590));
#776=EDGE_LOOP('',(#2591,#2592,#2593,#2594,#2595,#2596,#2597,#2598,#2599,
#2600,#2601,#2602,#2603,#2604,#2605,#2606,#2607,#2608,#2609,#2610,#2611));
#777=EDGE_LOOP('',(#2612));
#778=EDGE_LOOP('',(#2613,#2614,#2615,#2616));
#779=EDGE_LOOP('',(#2617,#2618,#2619,#2620,#2621));
#780=EDGE_LOOP('',(#2622,#2623,#2624,#2625,#2626));
#781=EDGE_LOOP('',(#2627,#2628,#2629,#2630,#2631));
#782=EDGE_LOOP('',(#2632,#2633,#2634,#2635));
#783=EDGE_LOOP('',(#2636,#2637,#2638,#2639));
#784=EDGE_LOOP('',(#2640,#2641,#2642,#2643,#2644));
#785=EDGE_LOOP('',(#2645,#2646,#2647,#2648));
#786=EDGE_LOOP('',(#2649,#2650,#2651,#2652,#2653));
#787=EDGE_LOOP('',(#2654,#2655,#2656,#2657,#2658));
#788=EDGE_LOOP('',(#2659));
#789=EDGE_LOOP('',(#2660,#2661,#2662,#2663,#2664,#2665,#2666,#2667,#2668,
#2669,#2670,#2671,#2672,#2673,#2674,#2675,#2676,#2677,#2678,#2679,#2680,
#2681,#2682));
#790=EDGE_LOOP('',(#2683,#2684,#2685,#2686));
#791=EDGE_LOOP('',(#2687));
#792=EDGE_LOOP('',(#2688));
#793=EDGE_LOOP('',(#2689));
#794=EDGE_LOOP('',(#2690));
#795=EDGE_LOOP('',(#2691));
#796=EDGE_LOOP('',(#2692));
#797=EDGE_LOOP('',(#2693));
#798=EDGE_LOOP('',(#2694));
#799=EDGE_LOOP('',(#2695));
#800=EDGE_LOOP('',(#2696));
#801=EDGE_LOOP('',(#2697));
#802=EDGE_LOOP('',(#2698));
#803=EDGE_LOOP('',(#2699,#2700,#2701,#2702));
#804=EDGE_LOOP('',(#2703,#2704,#2705,#2706,#2707,#2708,#2709,#2710));
#805=EDGE_LOOP('',(#2711,#2712,#2713,#2714,#2715,#2716,#2717,#2718));
#806=EDGE_LOOP('',(#2719,#2720,#2721,#2722,#2723,#2724,#2725,#2726));
#807=EDGE_LOOP('',(#2727,#2728,#2729,#2730,#2731,#2732,#2733,#2734));
#808=EDGE_LOOP('',(#2735,#2736,#2737,#2738,#2739,#2740,#2741,#2742));
#809=EDGE_LOOP('',(#2743,#2744,#2745,#2746,#2747,#2748,#2749,#2750));
#810=EDGE_LOOP('',(#2751,#2752,#2753,#2754,#2755,#2756,#2757,#2758));
#811=EDGE_LOOP('',(#2759,#2760,#2761,#2762,#2763,#2764,#2765,#2766));
#812=EDGE_LOOP('',(#2767,#2768,#2769,#2770,#2771,#2772,#2773,#2774));
#813=EDGE_LOOP('',(#2775,#2776,#2777,#2778,#2779,#2780,#2781,#2782));
#814=EDGE_LOOP('',(#2783,#2784,#2785,#2786,#2787,#2788,#2789,#2790,#2791,
#2792,#2793,#2794,#2795,#2796,#2797,#2798,#2799,#2800,#2801,#2802,#2803));
#815=EDGE_LOOP('',(#2804));
#816=EDGE_LOOP('',(#2805,#2806,#2807,#2808));
#817=EDGE_LOOP('',(#2809,#2810,#2811,#2812,#2813));
#818=EDGE_LOOP('',(#2814,#2815,#2816,#2817,#2818));
#819=EDGE_LOOP('',(#2819,#2820,#2821,#2822,#2823));
#820=EDGE_LOOP('',(#2824,#2825,#2826,#2827));
#821=EDGE_LOOP('',(#2828,#2829,#2830,#2831));
#822=EDGE_LOOP('',(#2832,#2833,#2834,#2835,#2836));
#823=EDGE_LOOP('',(#2837,#2838,#2839,#2840));
#824=EDGE_LOOP('',(#2841,#2842,#2843,#2844,#2845));
#825=EDGE_LOOP('',(#2846,#2847,#2848,#2849,#2850));
#826=EDGE_LOOP('',(#2851));
#827=EDGE_LOOP('',(#2852));
#828=EDGE_LOOP('',(#2853));
#829=EDGE_LOOP('',(#2854));
#830=EDGE_LOOP('',(#2855));
#831=EDGE_LOOP('',(#2856));
#832=EDGE_LOOP('',(#2857));
#833=EDGE_LOOP('',(#2858));
#834=EDGE_LOOP('',(#2859));
#835=EDGE_LOOP('',(#2860));
#836=EDGE_LOOP('',(#2861));
#837=EDGE_LOOP('',(#2862));
#838=EDGE_LOOP('',(#2863,#2864,#2865,#2866));
#839=EDGE_LOOP('',(#2867));
#840=EDGE_LOOP('',(#2868,#2869,#2870,#2871,#2872,#2873,#2874,#2875,#2876,
#2877,#2878,#2879,#2880,#2881,#2882,#2883,#2884,#2885,#2886,#2887,#2888,
#2889,#2890));
#841=EDGE_LOOP('',(#2891,#2892,#2893,#2894));
#842=EDGE_LOOP('',(#2895,#2896));
#843=EDGE_LOOP('',(#2897,#2898));
#844=EDGE_LOOP('',(#2899,#2900));
#845=EDGE_LOOP('',(#2901,#2902));
#846=EDGE_LOOP('',(#2903,#2904));
#847=EDGE_LOOP('',(#2905,#2906));
#848=EDGE_LOOP('',(#2907,#2908));
#849=EDGE_LOOP('',(#2909,#2910));
#850=EDGE_LOOP('',(#2911,#2912));
#851=EDGE_LOOP('',(#2913,#2914));
#852=EDGE_LOOP('',(#2915,#2916,#2917,#2918));
#853=EDGE_LOOP('',(#2919,#2920,#2921,#2922));
#854=EDGE_LOOP('',(#2923));
#855=EDGE_LOOP('',(#2924));
#856=EDGE_LOOP('',(#2925));
#857=EDGE_LOOP('',(#2926));
#858=EDGE_LOOP('',(#2927,#2928,#2929,#2930,#2931,#2932,#2933,#2934,#2935));
#859=EDGE_LOOP('',(#2936,#2937,#2938,#2939,#2940,#2941,#2942,#2943,#2944));
#860=EDGE_LOOP('',(#2945,#2946,#2947,#2948));
#861=EDGE_LOOP('',(#2949,#2950,#2951,#2952));
#862=EDGE_LOOP('',(#2953,#2954,#2955,#2956));
#863=EDGE_LOOP('',(#2957,#2958,#2959,#2960));
#864=EDGE_LOOP('',(#2961,#2962,#2963,#2964));
#865=EDGE_LOOP('',(#2965,#2966,#2967,#2968));
#866=EDGE_LOOP('',(#2969,#2970,#2971,#2972));
#867=EDGE_LOOP('',(#2973));
#868=EDGE_LOOP('',(#2974));
#869=EDGE_LOOP('',(#2975));
#870=EDGE_LOOP('',(#2976));
#871=EDGE_LOOP('',(#2977,#2978,#2979,#2980));
#872=EDGE_LOOP('',(#2981,#2982,#2983,#2984));
#873=EDGE_LOOP('',(#2985,#2986,#2987,#2988));
#874=EDGE_LOOP('',(#2989,#2990,#2991,#2992,#2993,#2994,#2995,#2996,#2997,
#2998));
#875=EDGE_LOOP('',(#2999,#3000,#3001,#3002));
#876=EDGE_LOOP('',(#3003,#3004,#3005,#3006));
#877=EDGE_LOOP('',(#3007,#3008,#3009,#3010,#3011,#3012,#3013,#3014,#3015,
#3016));
#878=EDGE_LOOP('',(#3017,#3018,#3019,#3020));
#879=EDGE_LOOP('',(#3021,#3022,#3023,#3024));
#880=EDGE_LOOP('',(#3025,#3026,#3027,#3028));
#881=EDGE_LOOP('',(#3029,#3030,#3031,#3032,#3033,#3034));
#882=EDGE_LOOP('',(#3035,#3036,#3037,#3038,#3039,#3040,#3041,#3042,#3043,
#3044,#3045,#3046));
#883=EDGE_LOOP('',(#3047));
#884=EDGE_LOOP('',(#3048,#3049,#3050,#3051,#3052,#3053));
#885=EDGE_LOOP('',(#3054,#3055,#3056,#3057));
#886=EDGE_LOOP('',(#3058,#3059,#3060,#3061));
#887=EDGE_LOOP('',(#3062,#3063,#3064,#3065));
#888=EDGE_LOOP('',(#3066,#3067,#3068,#3069));
#889=EDGE_LOOP('',(#3070,#3071,#3072,#3073));
#890=EDGE_LOOP('',(#3074,#3075,#3076,#3077));
#891=EDGE_LOOP('',(#3078));
#892=EDGE_LOOP('',(#3079,#3080,#3081,#3082));
#893=EDGE_LOOP('',(#3083,#3084,#3085,#3086));
#894=EDGE_LOOP('',(#3087));
#895=EDGE_LOOP('',(#3088));
#896=EDGE_LOOP('',(#3089));
#897=EDGE_LOOP('',(#3090));
#898=EDGE_LOOP('',(#3091,#3092,#3093,#3094));
#899=EDGE_LOOP('',(#3095));
#900=EDGE_LOOP('',(#3096));
#901=EDGE_LOOP('',(#3097));
#902=EDGE_LOOP('',(#3098,#3099,#3100,#3101));
#903=EDGE_LOOP('',(#3102));
#904=EDGE_LOOP('',(#3103,#3104,#3105,#3106));
#905=EDGE_LOOP('',(#3107));
#906=EDGE_LOOP('',(#3108));
#907=EDGE_LOOP('',(#3109,#3110,#3111,#3112));
#908=EDGE_LOOP('',(#3113,#3114,#3115,#3116));
#909=EDGE_LOOP('',(#3117));
#910=EDGE_LOOP('',(#3118));
#911=EDGE_LOOP('',(#3119));
#912=EDGE_LOOP('',(#3120));
#913=EDGE_LOOP('',(#3121,#3122,#3123,#3124));
#914=EDGE_LOOP('',(#3125,#3126,#3127,#3128));
#915=EDGE_LOOP('',(#3129));
#916=EDGE_LOOP('',(#3130));
#917=EDGE_LOOP('',(#3131));
#918=EDGE_LOOP('',(#3132));
#919=EDGE_LOOP('',(#3133,#3134,#3135,#3136));
#920=EDGE_LOOP('',(#3137,#3138,#3139,#3140));
#921=EDGE_LOOP('',(#3141,#3142,#3143,#3144));
#922=EDGE_LOOP('',(#3145,#3146,#3147,#3148));
#923=EDGE_LOOP('',(#3149,#3150,#3151,#3152));
#924=EDGE_LOOP('',(#3153,#3154,#3155,#3156));
#925=EDGE_LOOP('',(#3157,#3158,#3159,#3160,#3161,#3162));
#926=EDGE_LOOP('',(#3163,#3164,#3165,#3166,#3167,#3168));
#927=EDGE_LOOP('',(#3169));
#928=EDGE_LOOP('',(#3170));
#929=EDGE_LOOP('',(#3171,#3172,#3173,#3174));
#930=EDGE_LOOP('',(#3175,#3176,#3177,#3178));
#931=EDGE_LOOP('',(#3179,#3180,#3181,#3182));
#932=EDGE_LOOP('',(#3183));
#933=EDGE_LOOP('',(#3184));
#934=EDGE_LOOP('',(#3185,#3186,#3187,#3188));
#935=EDGE_LOOP('',(#3189,#3190,#3191,#3192));
#936=EDGE_LOOP('',(#3193,#3194,#3195,#3196));
#937=EDGE_LOOP('',(#3197));
#938=EDGE_LOOP('',(#3198));
#939=EDGE_LOOP('',(#3199,#3200,#3201,#3202));
#940=EDGE_LOOP('',(#3203));
#941=EDGE_LOOP('',(#3204));
#942=EDGE_LOOP('',(#3205,#3206,#3207,#3208));
#943=EDGE_LOOP('',(#3209,#3210,#3211,#3212));
#944=EDGE_LOOP('',(#3213));
#945=EDGE_LOOP('',(#3214));
#946=EDGE_LOOP('',(#3215));
#947=EDGE_LOOP('',(#3216));
#948=EDGE_LOOP('',(#3217,#3218,#3219,#3220,#3221,#3222));
#949=EDGE_LOOP('',(#3223,#3224,#3225,#3226,#3227));
#950=EDGE_LOOP('',(#3228,#3229,#3230,#3231));
#951=EDGE_LOOP('',(#3232,#3233,#3234,#3235));
#952=EDGE_LOOP('',(#3236));
#953=EDGE_LOOP('',(#3237));
#954=EDGE_LOOP('',(#3238,#3239,#3240,#3241,#3242));
#955=EDGE_LOOP('',(#3243));
#956=EDGE_LOOP('',(#3244));
#957=EDGE_LOOP('',(#3245,#3246,#3247,#3248));
#958=EDGE_LOOP('',(#3249,#3250,#3251,#3252,#3253,#3254));
#959=EDGE_LOOP('',(#3255,#3256,#3257,#3258,#3259));
#960=EDGE_LOOP('',(#3260));
#961=EDGE_LOOP('',(#3261));
#962=EDGE_LOOP('',(#3262,#3263,#3264,#3265));
#963=EDGE_LOOP('',(#3266,#3267,#3268,#3269));
#964=EDGE_LOOP('',(#3270,#3271,#3272,#3273));
#965=EDGE_LOOP('',(#3274));
#966=EDGE_LOOP('',(#3275));
#967=EDGE_LOOP('',(#3276,#3277,#3278,#3279,#3280));
#968=EDGE_LOOP('',(#3281,#3282));
#969=EDGE_LOOP('',(#3283,#3284));
#970=EDGE_LOOP('',(#3285,#3286));
#971=EDGE_LOOP('',(#3287,#3288));
#972=EDGE_LOOP('',(#3289,#3290));
#973=EDGE_LOOP('',(#3291,#3292));
#974=EDGE_LOOP('',(#3293,#3294));
#975=EDGE_LOOP('',(#3295,#3296,#3297,#3298));
#976=EDGE_LOOP('',(#3299,#3300,#3301,#3302,#3303,#3304,#3305,#3306,#3307,
#3308,#3309,#3310,#3311,#3312,#3313,#3314,#3315,#3316));
#977=EDGE_LOOP('',(#3317,#3318,#3319,#3320));
#978=EDGE_LOOP('',(#3321,#3322,#3323,#3324));
#979=EDGE_LOOP('',(#3325,#3326,#3327,#3328));
#980=EDGE_LOOP('',(#3329,#3330,#3331,#3332));
#981=EDGE_LOOP('',(#3333,#3334,#3335,#3336,#3337,#3338));
#982=EDGE_LOOP('',(#3339,#3340,#3341,#3342));
#983=EDGE_LOOP('',(#3343,#3344,#3345,#3346));
#984=EDGE_LOOP('',(#3347,#3348,#3349,#3350));
#985=EDGE_LOOP('',(#3351,#3352,#3353,#3354));
#986=EDGE_LOOP('',(#3355,#3356,#3357,#3358));
#987=EDGE_LOOP('',(#3359,#3360,#3361,#3362,#3363,#3364,#3365,#3366,#3367,
#3368,#3369,#3370,#3371,#3372,#3373,#3374,#3375,#3376));
#988=EDGE_LOOP('',(#3377,#3378,#3379,#3380));
#989=EDGE_LOOP('',(#3381,#3382,#3383,#3384));
#990=EDGE_LOOP('',(#3385));
#991=EDGE_LOOP('',(#3386));
#992=EDGE_LOOP('',(#3387,#3388,#3389,#3390));
#993=EDGE_LOOP('',(#3391));
#994=EDGE_LOOP('',(#3392));
#995=EDGE_LOOP('',(#3393,#3394,#3395,#3396));
#996=EDGE_LOOP('',(#3397));
#997=EDGE_LOOP('',(#3398));
#998=EDGE_LOOP('',(#3399,#3400,#3401,#3402));
#999=EDGE_LOOP('',(#3403));
#1000=EDGE_LOOP('',(#3404));
#1001=EDGE_LOOP('',(#3405,#3406,#3407,#3408));
#1002=EDGE_LOOP('',(#3409));
#1003=EDGE_LOOP('',(#3410));
#1004=EDGE_LOOP('',(#3411,#3412,#3413,#3414));
#1005=EDGE_LOOP('',(#3415,#3416,#3417,#3418));
#1006=EDGE_LOOP('',(#3419,#3420,#3421,#3422));
#1007=EDGE_LOOP('',(#3423));
#1008=EDGE_LOOP('',(#3424));
#1009=EDGE_LOOP('',(#3425));
#1010=EDGE_LOOP('',(#3426));
#1011=LINE('',#5705,#1166);
#1012=LINE('',#5711,#1167);
#1013=LINE('',#5717,#1168);
#1014=LINE('',#5723,#1169);
#1015=LINE('',#5729,#1170);
#1016=LINE('',#5734,#1171);
#1017=LINE('',#5736,#1172);
#1018=LINE('',#5738,#1173);
#1019=LINE('',#5739,#1174);
#1020=LINE('',#5742,#1175);
#1021=LINE('',#5744,#1176);
#1022=LINE('',#5745,#1177);
#1023=LINE('',#5748,#1178);
#1024=LINE('',#5750,#1179);
#1025=LINE('',#5751,#1180);
#1026=LINE('',#5753,#1181);
#1027=LINE('',#5754,#1182);
#1028=LINE('',#5762,#1183);
#1029=LINE('',#5773,#1184);
#1030=LINE('',#5781,#1185);
#1031=LINE('',#5784,#1186);
#1032=LINE('',#5793,#1187);
#1033=LINE('',#5840,#1188);
#1034=LINE('',#5884,#1189);
#1035=LINE('',#5928,#1190);
#1036=LINE('',#5975,#1191);
#1037=LINE('',#6022,#1192);
#1038=LINE('',#6069,#1193);
#1039=LINE('',#6113,#1194);
#1040=LINE('',#6157,#1195);
#1041=LINE('',#6204,#1196);
#1042=LINE('',#6286,#1197);
#1043=LINE('',#6291,#1198);
#1044=LINE('',#6324,#1199);
#1045=LINE('',#6381,#1200);
#1046=LINE('',#6406,#1201);
#1047=LINE('',#6473,#1202);
#1048=LINE('',#6520,#1203);
#1049=LINE('',#6567,#1204);
#1050=LINE('',#6610,#1205);
#1051=LINE('',#6654,#1206);
#1052=LINE('',#6692,#1207);
#1053=LINE('',#6731,#1208);
#1054=LINE('',#6792,#1209);
#1055=LINE('',#6795,#1210);
#1056=LINE('',#6845,#1211);
#1057=LINE('',#6851,#1212);
#1058=LINE('',#6867,#1213);
#1059=LINE('',#6888,#1214);
#1060=LINE('',#6913,#1215);
#1061=LINE('',#6914,#1216);
#1062=LINE('',#6916,#1217);
#1063=LINE('',#6918,#1218);
#1064=LINE('',#6923,#1219);
#1065=LINE('',#6926,#1220);
#1066=LINE('',#6928,#1221);
#1067=LINE('',#6943,#1222);
#1068=LINE('',#6950,#1223);
#1069=LINE('',#6953,#1224);
#1070=LINE('',#6957,#1225);
#1071=LINE('',#6961,#1226);
#1072=LINE('',#6965,#1227);
#1073=LINE('',#6967,#1228);
#1074=LINE('',#6969,#1229);
#1075=LINE('',#6971,#1230);
#1076=LINE('',#6973,#1231);
#1077=LINE('',#6975,#1232);
#1078=LINE('',#6977,#1233);
#1079=LINE('',#6979,#1234);
#1080=LINE('',#6980,#1235);
#1081=LINE('',#6983,#1236);
#1082=LINE('',#6984,#1237);
#1083=LINE('',#6987,#1238);
#1084=LINE('',#6988,#1239);
#1085=LINE('',#6991,#1240);
#1086=LINE('',#6993,#1241);
#1087=LINE('',#6995,#1242);
#1088=LINE('',#6997,#1243);
#1089=LINE('',#6999,#1244);
#1090=LINE('',#7001,#1245);
#1091=LINE('',#7003,#1246);
#1092=LINE('',#7005,#1247);
#1093=LINE('',#7006,#1248);
#1094=LINE('',#7009,#1249);
#1095=LINE('',#7010,#1250);
#1096=LINE('',#7013,#1251);
#1097=LINE('',#7014,#1252);
#1098=LINE('',#7017,#1253);
#1099=LINE('',#7018,#1254);
#1100=LINE('',#7020,#1255);
#1101=LINE('',#7022,#1256);
#1102=LINE('',#7024,#1257);
#1103=LINE('',#7026,#1258);
#1104=LINE('',#7027,#1259);
#1105=LINE('',#7028,#1260);
#1106=LINE('',#7031,#1261);
#1107=LINE('',#7032,#1262);
#1108=LINE('',#7033,#1263);
#1109=LINE('',#7036,#1264);
#1110=LINE('',#7039,#1265);
#1111=LINE('',#7041,#1266);
#1112=LINE('',#7048,#1267);
#1113=LINE('',#7054,#1268);
#1114=LINE('',#7063,#1269);
#1115=LINE('',#7073,#1270);
#1116=LINE('',#7079,#1271);
#1117=LINE('',#7086,#1272);
#1118=LINE('',#7092,#1273);
#1119=LINE('',#7101,#1274);
#1120=LINE('',#7107,#1275);
#1121=LINE('',#7115,#1276);
#1122=LINE('',#7117,#1277);
#1123=LINE('',#7119,#1278);
#1124=LINE('',#7120,#1279);
#1125=LINE('',#7123,#1280);
#1126=LINE('',#7125,#1281);
#1127=LINE('',#7126,#1282);
#1128=LINE('',#7129,#1283);
#1129=LINE('',#7131,#1284);
#1130=LINE('',#7132,#1285);
#1131=LINE('',#7135,#1286);
#1132=LINE('',#7137,#1287);
#1133=LINE('',#7138,#1288);
#1134=LINE('',#7141,#1289);
#1135=LINE('',#7143,#1290);
#1136=LINE('',#7144,#1291);
#1137=LINE('',#7146,#1292);
#1138=LINE('',#7147,#1293);
#1139=LINE('',#7159,#1294);
#1140=LINE('',#7163,#1295);
#1141=LINE('',#7167,#1296);
#1142=LINE('',#7174,#1297);
#1143=LINE('',#7176,#1298);
#1144=LINE('',#7190,#1299);
#1145=LINE('',#7199,#1300);
#1146=LINE('',#7205,#1301);
#1147=LINE('',#7210,#1302);
#1148=LINE('',#7228,#1303);
#1149=LINE('',#7234,#1304);
#1150=LINE('',#7238,#1305);
#1151=LINE('',#7244,#1306);
#1152=LINE('',#7249,#1307);
#1153=LINE('',#7264,#1308);
#1154=LINE('',#7273,#1309);
#1155=LINE('',#7277,#1310);
#1156=LINE('',#7281,#1311);
#1157=LINE('',#7284,#1312);
#1158=LINE('',#7420,#1313);
#1159=LINE('',#7673,#1314);
#1160=LINE('',#7715,#1315);
#1161=LINE('',#7720,#1316);
#1162=LINE('',#7729,#1317);
#1163=LINE('',#7734,#1318);
#1164=LINE('',#7745,#1319);
#1165=LINE('',#7751,#1320);
#1166=VECTOR('',#4499,0.75);
#1167=VECTOR('',#4506,0.425);
#1168=VECTOR('',#4513,0.425);
#1169=VECTOR('',#4520,0.425);
#1170=VECTOR('',#4527,0.425);
#1171=VECTOR('',#4532,1.);
#1172=VECTOR('',#4533,1.);
#1173=VECTOR('',#4534,1.);
#1174=VECTOR('',#4535,1.);
#1175=VECTOR('',#4538,1.);
#1176=VECTOR('',#4539,1.);
#1177=VECTOR('',#4540,1.);
#1178=VECTOR('',#4543,1.);
#1179=VECTOR('',#4544,1.);
#1180=VECTOR('',#4545,1.);
#1181=VECTOR('',#4548,1.);
#1182=VECTOR('',#4549,1.);
#1183=VECTOR('',#4560,0.4);
#1184=VECTOR('',#4575,1.2);
#1185=VECTOR('',#4586,0.75);
#1186=VECTOR('',#4589,0.6);
#1187=VECTOR('',#4602,0.22);
#1188=VECTOR('',#4611,0.22);
#1189=VECTOR('',#4622,0.22);
#1190=VECTOR('',#4633,0.22);
#1191=VECTOR('',#4642,0.22);
#1192=VECTOR('',#4651,0.22);
#1193=VECTOR('',#4660,0.22);
#1194=VECTOR('',#4671,0.22);
#1195=VECTOR('',#4682,0.22);
#1196=VECTOR('',#4691,0.22);
#1197=VECTOR('',#4768,1.4);
#1198=VECTOR('',#4775,0.75);
#1199=VECTOR('',#4782,0.22);
#1200=VECTOR('',#4793,0.22);
#1201=VECTOR('',#4802,0.22);
#1202=VECTOR('',#4815,0.22);
#1203=VECTOR('',#4824,0.22);
#1204=VECTOR('',#4833,0.22);
#1205=VECTOR('',#4842,0.22);
#1206=VECTOR('',#4853,0.22);
#1207=VECTOR('',#4862,0.22);
#1208=VECTOR('',#4871,0.22);
#1209=VECTOR('',#4950,1.4);
#1210=VECTOR('',#4955,0.8);
#1211=VECTOR('',#5010,0.42);
#1212=VECTOR('',#5017,0.8);
#1213=VECTOR('',#5028,0.734027674973257);
#1214=VECTOR('',#5035,0.734027674973257);
#1215=VECTOR('',#5038,1.);
#1216=VECTOR('',#5039,1.);
#1217=VECTOR('',#5042,1.);
#1218=VECTOR('',#5045,1.);
#1219=VECTOR('',#5050,0.4);
#1220=VECTOR('',#5055,1.);
#1221=VECTOR('',#5058,1.);
#1222=VECTOR('',#5083,0.8);
#1223=VECTOR('',#5090,1.);
#1224=VECTOR('',#5093,1.);
#1225=VECTOR('',#5096,1.);
#1226=VECTOR('',#5099,1.);
#1227=VECTOR('',#5104,1.);
#1228=VECTOR('',#5105,1.);
#1229=VECTOR('',#5106,1.);
#1230=VECTOR('',#5107,1.);
#1231=VECTOR('',#5108,1.);
#1232=VECTOR('',#5109,1.);
#1233=VECTOR('',#5110,1.);
#1234=VECTOR('',#5111,1.);
#1235=VECTOR('',#5112,1.);
#1236=VECTOR('',#5115,1.);
#1237=VECTOR('',#5116,1.);
#1238=VECTOR('',#5119,1.);
#1239=VECTOR('',#5120,1.);
#1240=VECTOR('',#5123,1.);
#1241=VECTOR('',#5124,1.);
#1242=VECTOR('',#5125,1.);
#1243=VECTOR('',#5126,1.);
#1244=VECTOR('',#5127,1.);
#1245=VECTOR('',#5128,1.);
#1246=VECTOR('',#5129,1.);
#1247=VECTOR('',#5130,1.);
#1248=VECTOR('',#5131,1.);
#1249=VECTOR('',#5134,1.);
#1250=VECTOR('',#5135,1.);
#1251=VECTOR('',#5138,1.);
#1252=VECTOR('',#5139,1.);
#1253=VECTOR('',#5142,1.);
#1254=VECTOR('',#5143,1.);
#1255=VECTOR('',#5146,1.);
#1256=VECTOR('',#5149,1.);
#1257=VECTOR('',#5150,1.);
#1258=VECTOR('',#5151,1.);
#1259=VECTOR('',#5152,1.);
#1260=VECTOR('',#5153,1.);
#1261=VECTOR('',#5156,1.);
#1262=VECTOR('',#5157,1.);
#1263=VECTOR('',#5158,1.);
#1264=VECTOR('',#5163,1.);
#1265=VECTOR('',#5168,1.);
#1266=VECTOR('',#5171,1.);
#1267=VECTOR('',#5180,0.605);
#1268=VECTOR('',#5187,0.8);
#1269=VECTOR('',#5200,0.165);
#1270=VECTOR('',#5213,0.9);
#1271=VECTOR('',#5222,0.6);
#1272=VECTOR('',#5231,0.605);
#1273=VECTOR('',#5238,0.8);
#1274=VECTOR('',#5251,0.225);
#1275=VECTOR('',#5258,0.8);
#1276=VECTOR('',#5269,1.);
#1277=VECTOR('',#5270,1.);
#1278=VECTOR('',#5271,1.);
#1279=VECTOR('',#5272,1.);
#1280=VECTOR('',#5275,1.);
#1281=VECTOR('',#5276,1.);
#1282=VECTOR('',#5277,1.);
#1283=VECTOR('',#5280,1.);
#1284=VECTOR('',#5281,1.);
#1285=VECTOR('',#5282,1.);
#1286=VECTOR('',#5285,1.);
#1287=VECTOR('',#5286,1.);
#1288=VECTOR('',#5287,1.);
#1289=VECTOR('',#5290,1.);
#1290=VECTOR('',#5291,1.);
#1291=VECTOR('',#5292,1.);
#1292=VECTOR('',#5295,1.);
#1293=VECTOR('',#5296,1.);
#1294=VECTOR('',#5313,0.325);
#1295=VECTOR('',#5318,0.35);
#1296=VECTOR('',#5323,0.335);
#1297=VECTOR('',#5332,0.21);
#1298=VECTOR('',#5335,0.2);
#1299=VECTOR('',#5358,1.6);
#1300=VECTOR('',#5369,1.6);
#1301=VECTOR('',#5378,0.62);
#1302=VECTOR('',#5383,3.75);
#1303=VECTOR('',#5408,1.070235);
#1304=VECTOR('',#5415,0.6);
#1305=VECTOR('',#5420,0.63);
#1306=VECTOR('',#5429,1.070235);
#1307=VECTOR('',#5436,0.63);
#1308=VECTOR('',#5455,1.129765);
#1309=VECTOR('',#5466,1.57);
#1310=VECTOR('',#5471,1.6);
#1311=VECTOR('',#5476,1.57);
#1312=VECTOR('',#5481,1.129765);
#1313=VECTOR('',#5528,1.123812);
#1314=VECTOR('',#5597,1.076188);
#1315=VECTOR('',#5626,1.119765);
#1316=VECTOR('',#5633,1.085235);
#1317=VECTOR('',#5644,1.119765);
#1318=VECTOR('',#5651,1.085235);
#1319=VECTOR('',#5668,1.2);
#1320=VECTOR('',#5675,1.6);
#1321=CIRCLE('',#3966,0.75);
#1322=CIRCLE('',#3967,0.75);
#1323=CIRCLE('',#3969,0.425);
#1324=CIRCLE('',#3970,0.425);
#1325=CIRCLE('',#3972,0.425);
#1326=CIRCLE('',#3973,0.425);
#1327=CIRCLE('',#3975,0.425);
#1328=CIRCLE('',#3976,0.425);
#1329=CIRCLE('',#3978,0.425);
#1330=CIRCLE('',#3979,0.425);
#1331=CIRCLE('',#3988,0.4);
#1332=CIRCLE('',#3989,0.4);
#1333=CIRCLE('',#3992,1.2);
#1334=CIRCLE('',#3993,0.75);
#1335=CIRCLE('',#3995,1.2);
#1336=CIRCLE('',#3998,0.75);
#1337=CIRCLE('',#3999,0.6);
#1338=CIRCLE('',#4002,0.6);
#1339=CIRCLE('',#4007,0.22);
#1340=CIRCLE('',#4008,0.22);
#1341=CIRCLE('',#4009,0.22);
#1342=CIRCLE('',#4011,0.22);
#1343=CIRCLE('',#4012,0.22);
#1344=CIRCLE('',#4013,0.22);
#1345=CIRCLE('',#4014,0.22);
#1346=CIRCLE('',#4016,0.22);
#1347=CIRCLE('',#4017,0.22);
#1348=CIRCLE('',#4018,0.22);
#1349=CIRCLE('',#4019,0.22);
#1350=CIRCLE('',#4021,0.22);
#1351=CIRCLE('',#4022,0.22);
#1352=CIRCLE('',#4023,0.22);
#1353=CIRCLE('',#4025,0.22);
#1354=CIRCLE('',#4026,0.22);
#1355=CIRCLE('',#4027,0.22);
#1356=CIRCLE('',#4029,0.22);
#1357=CIRCLE('',#4030,0.22);
#1358=CIRCLE('',#4031,0.22);
#1359=CIRCLE('',#4033,0.22);
#1360=CIRCLE('',#4034,0.22);
#1361=CIRCLE('',#4035,0.22);
#1362=CIRCLE('',#4036,0.22);
#1363=CIRCLE('',#4038,0.22);
#1364=CIRCLE('',#4039,0.22);
#1365=CIRCLE('',#4040,0.22);
#1366=CIRCLE('',#4041,0.22);
#1367=CIRCLE('',#4043,0.22);
#1368=CIRCLE('',#4044,0.22);
#1369=CIRCLE('',#4045,0.22);
#1370=CIRCLE('',#4047,0.22);
#1371=CIRCLE('',#4048,0.22);
#1372=CIRCLE('',#4049,0.22);
#1373=CIRCLE('',#4051,0.917615790157152);
#1374=CIRCLE('',#4052,0.917615790157152);
#1375=CIRCLE('',#4053,0.917615790157152);
#1376=CIRCLE('',#4054,0.917615790157152);
#1377=CIRCLE('',#4055,0.917615790157152);
#1378=CIRCLE('',#4056,0.917615790157152);
#1379=CIRCLE('',#4057,0.917615790157152);
#1380=CIRCLE('',#4058,0.917615790157152);
#1381=CIRCLE('',#4059,0.917615790157152);
#1382=CIRCLE('',#4060,0.917615790157152);
#1383=CIRCLE('',#4061,0.75);
#1384=CIRCLE('',#4063,1.28238420984285);
#1385=CIRCLE('',#4065,1.28238420984285);
#1386=CIRCLE('',#4067,1.28238420984285);
#1387=CIRCLE('',#4069,1.28238420984285);
#1388=CIRCLE('',#4071,1.28238420984285);
#1389=CIRCLE('',#4073,1.28238420984285);
#1390=CIRCLE('',#4075,1.28238420984285);
#1391=CIRCLE('',#4077,1.28238420984285);
#1392=CIRCLE('',#4079,1.28238420984285);
#1393=CIRCLE('',#4081,1.28238420984285);
#1394=CIRCLE('',#4083,1.4);
#1395=CIRCLE('',#4085,1.4);
#1396=CIRCLE('',#4087,0.75);
#1397=CIRCLE('',#4091,0.22);
#1398=CIRCLE('',#4092,0.22);
#1399=CIRCLE('',#4093,0.22);
#1400=CIRCLE('',#4095,0.22);
#1401=CIRCLE('',#4096,0.22);
#1402=CIRCLE('',#4097,0.22);
#1403=CIRCLE('',#4098,0.22);
#1404=CIRCLE('',#4100,0.22);
#1405=CIRCLE('',#4101,0.22);
#1406=CIRCLE('',#4102,0.22);
#1407=CIRCLE('',#4103,0.22);
#1408=CIRCLE('',#4105,0.22);
#1409=CIRCLE('',#4106,0.22);
#1410=CIRCLE('',#4107,0.22);
#1411=CIRCLE('',#4109,0.22);
#1412=CIRCLE('',#4110,0.22);
#1413=CIRCLE('',#4111,0.22);
#1414=CIRCLE('',#4113,0.22);
#1415=CIRCLE('',#4114,0.22);
#1416=CIRCLE('',#4115,0.22);
#1417=CIRCLE('',#4117,0.22);
#1418=CIRCLE('',#4118,0.22);
#1419=CIRCLE('',#4119,0.22);
#1420=CIRCLE('',#4120,0.22);
#1421=CIRCLE('',#4122,0.22);
#1422=CIRCLE('',#4123,0.22);
#1423=CIRCLE('',#4124,0.22);
#1424=CIRCLE('',#4125,0.22);
#1425=CIRCLE('',#4127,0.22);
#1426=CIRCLE('',#4128,0.22);
#1427=CIRCLE('',#4129,0.22);
#1428=CIRCLE('',#4131,0.22);
#1429=CIRCLE('',#4132,0.22);
#1430=CIRCLE('',#4133,0.22);
#1431=CIRCLE('',#4135,0.917615790157152);
#1432=CIRCLE('',#4136,0.917615790157152);
#1433=CIRCLE('',#4137,0.917615790157152);
#1434=CIRCLE('',#4138,0.917615790157152);
#1435=CIRCLE('',#4139,0.917615790157152);
#1436=CIRCLE('',#4140,0.917615790157152);
#1437=CIRCLE('',#4141,0.917615790157152);
#1438=CIRCLE('',#4142,0.917615790157152);
#1439=CIRCLE('',#4143,0.917615790157152);
#1440=CIRCLE('',#4144,0.917615790157152);
#1441=CIRCLE('',#4145,0.8);
#1442=CIRCLE('',#4147,1.28238420984285);
#1443=CIRCLE('',#4149,1.28238420984285);
#1444=CIRCLE('',#4151,1.28238420984285);
#1445=CIRCLE('',#4153,1.28238420984285);
#1446=CIRCLE('',#4155,1.28238420984285);
#1447=CIRCLE('',#4157,1.28238420984285);
#1448=CIRCLE('',#4159,1.28238420984285);
#1449=CIRCLE('',#4161,1.28238420984285);
#1450=CIRCLE('',#4163,1.28238420984285);
#1451=CIRCLE('',#4165,1.28238420984285);
#1452=CIRCLE('',#4167,1.4);
#1453=CIRCLE('',#4168,0.8);
#1454=CIRCLE('',#4170,1.4);
#1455=CIRCLE('',#4175,0.2);
#1456=CIRCLE('',#4177,0.2);
#1457=CIRCLE('',#4179,0.2);
#1458=CIRCLE('',#4181,0.2);
#1459=CIRCLE('',#4183,0.2);
#1460=CIRCLE('',#4185,0.2);
#1461=CIRCLE('',#4187,0.2);
#1462=CIRCLE('',#4189,0.2);
#1463=CIRCLE('',#4191,0.2);
#1464=CIRCLE('',#4193,0.2);
#1465=CIRCLE('',#4199,0.42);
#1466=CIRCLE('',#4200,0.42);
#1467=CIRCLE('',#4202,0.8);
#1468=CIRCLE('',#4203,0.8);
#1469=CIRCLE('',#4208,0.6175);
#1470=CIRCLE('',#4210,0.6175);
#1471=CIRCLE('',#4215,0.338975);
#1472=CIRCLE('',#4216,0.338975);
#1473=CIRCLE('',#4230,0.8);
#1474=CIRCLE('',#4231,0.8);
#1475=CIRCLE('',#4233,0.6);
#1476=CIRCLE('',#4234,0.6);
#1477=CIRCLE('',#4236,0.6);
#1478=CIRCLE('',#4237,0.6);
#1479=CIRCLE('',#4256,0.605);
#1480=CIRCLE('',#4257,0.605);
#1481=CIRCLE('',#4259,0.8);
#1482=CIRCLE('',#4260,0.8);
#1483=CIRCLE('',#4265,0.165);
#1484=CIRCLE('',#4266,0.165);
#1485=CIRCLE('',#4269,0.9);
#1486=CIRCLE('',#4270,0.6);
#1487=CIRCLE('',#4272,0.9);
#1488=CIRCLE('',#4275,0.6);
#1489=CIRCLE('',#4279,0.605);
#1490=CIRCLE('',#4280,0.605);
#1491=CIRCLE('',#4282,0.8);
#1492=CIRCLE('',#4283,0.8);
#1493=CIRCLE('',#4288,0.225);
#1494=CIRCLE('',#4289,0.225);
#1495=CIRCLE('',#4291,0.8);
#1496=CIRCLE('',#4292,0.8);
#1497=CIRCLE('',#4305,0.1954);
#1498=CIRCLE('',#4307,0.3);
#1499=CIRCLE('',#4309,0.35);
#1500=CIRCLE('',#4311,0.35);
#1501=CIRCLE('',#4313,0.32);
#1502=CIRCLE('',#4315,0.22);
#1503=CIRCLE('',#4317,0.1954);
#1504=CIRCLE('',#4329,1.6);
#1505=CIRCLE('',#4330,1.6);
#1506=CIRCLE('',#4332,0.62);
#1507=CIRCLE('',#4334,1.6);
#1508=CIRCLE('',#4335,1.6);
#1509=CIRCLE('',#4337,0.62);
#1510=CIRCLE('',#4340,3.75);
#1511=CIRCLE('',#4341,3.75);
#1512=CIRCLE('',#4347,1.070235);
#1513=CIRCLE('',#4348,1.070235);
#1514=CIRCLE('',#4349,0.309556);
#1515=CIRCLE('',#4350,1.070235);
#1516=CIRCLE('',#4351,1.070235);
#1517=CIRCLE('',#4353,1.070235);
#1518=CIRCLE('',#4355,0.6);
#1519=CIRCLE('',#4356,0.6);
#1520=CIRCLE('',#4358,0.66);
#1521=CIRCLE('',#4361,1.070235);
#1522=CIRCLE('',#4363,0.66);
#1523=CIRCLE('',#4367,1.129765);
#1524=CIRCLE('',#4368,1.129765);
#1525=CIRCLE('',#4369,0.309556);
#1526=CIRCLE('',#4370,1.129765);
#1527=CIRCLE('',#4371,1.129765);
#1528=CIRCLE('',#4373,1.129765);
#1529=CIRCLE('',#4375,1.54);
#1530=CIRCLE('',#4376,1.129765);
#1531=CIRCLE('',#4378,1.6);
#1532=CIRCLE('',#4380,1.6);
#1533=CIRCLE('',#4382,1.54);
#1534=CIRCLE('',#4387,0.29765);
#1535=CIRCLE('',#4389,0.29765);
#1536=CIRCLE('',#4391,0.29765);
#1537=CIRCLE('',#4393,0.29765);
#1538=CIRCLE('',#4395,0.29765);
#1539=CIRCLE('',#4397,0.29765);
#1540=CIRCLE('',#4399,0.29765);
#1541=CIRCLE('',#4402,0.303778037777585);
#1542=CIRCLE('',#4403,0.303778037777585);
#1543=CIRCLE('',#4405,1.123812);
#1544=CIRCLE('',#4406,1.123812);
#1545=CIRCLE('',#4407,1.123812);
#1546=CIRCLE('',#4408,1.123812);
#1547=CIRCLE('',#4409,1.123812);
#1548=CIRCLE('',#4410,1.123812);
#1549=CIRCLE('',#4411,1.123812);
#1550=CIRCLE('',#4412,1.123812);
#1551=CIRCLE('',#4413,1.123812);
#1552=CIRCLE('',#4415,1.076188);
#1553=CIRCLE('',#4416,0.303778037777585);
#1554=CIRCLE('',#4418,0.303778037777585);
#1555=CIRCLE('',#4420,1.076188);
#1556=CIRCLE('',#4421,0.303778037777585);
#1557=CIRCLE('',#4423,0.303778037777585);
#1558=CIRCLE('',#4425,1.076188);
#1559=CIRCLE('',#4426,1.076188);
#1560=CIRCLE('',#4427,0.303778037777585);
#1561=CIRCLE('',#4429,0.303778037777585);
#1562=CIRCLE('',#4431,1.076188);
#1563=CIRCLE('',#4432,0.303778037777585);
#1564=CIRCLE('',#4434,0.303778037777585);
#1565=CIRCLE('',#4436,1.076188);
#1566=CIRCLE('',#4437,0.303778037777585);
#1567=CIRCLE('',#4439,0.303778037777585);
#1568=CIRCLE('',#4441,1.076188);
#1569=CIRCLE('',#4442,1.076188);
#1570=CIRCLE('',#4443,1.076188);
#1571=CIRCLE('',#4445,0.303778037777585);
#1572=CIRCLE('',#4447,0.303778037777585);
#1573=CIRCLE('',#4452,1.119765);
#1574=CIRCLE('',#4453,1.085235);
#1575=CIRCLE('',#4455,1.119765);
#1576=CIRCLE('',#4457,1.085235);
#1577=CIRCLE('',#4460,1.119765);
#1578=CIRCLE('',#4461,1.085235);
#1579=CIRCLE('',#4463,1.119765);
#1580=CIRCLE('',#4465,1.085235);
#1581=CIRCLE('',#4474,1.2);
#1582=CIRCLE('',#4475,1.2);
#1583=CIRCLE('',#4477,1.6);
#1584=CIRCLE('',#4478,1.6);
#1585=VERTEX_POINT('',#5702);
#1586=VERTEX_POINT('',#5704);
#1587=VERTEX_POINT('',#5708);
#1588=VERTEX_POINT('',#5710);
#1589=VERTEX_POINT('',#5714);
#1590=VERTEX_POINT('',#5716);
#1591=VERTEX_POINT('',#5720);
#1592=VERTEX_POINT('',#5722);
#1593=VERTEX_POINT('',#5726);
#1594=VERTEX_POINT('',#5728);
#1595=VERTEX_POINT('',#5732);
#1596=VERTEX_POINT('',#5733);
#1597=VERTEX_POINT('',#5735);
#1598=VERTEX_POINT('',#5737);
#1599=VERTEX_POINT('',#5741);
#1600=VERTEX_POINT('',#5743);
#1601=VERTEX_POINT('',#5747);
#1602=VERTEX_POINT('',#5749);
#1603=VERTEX_POINT('',#5759);
#1604=VERTEX_POINT('',#5761);
#1605=VERTEX_POINT('',#5766);
#1606=VERTEX_POINT('',#5768);
#1607=VERTEX_POINT('',#5771);
#1608=VERTEX_POINT('',#5776);
#1609=VERTEX_POINT('',#5778);
#1610=VERTEX_POINT('',#5783);
#1611=VERTEX_POINT('',#5790);
#1612=VERTEX_POINT('',#5792);
#1613=VERTEX_POINT('',#5794);
#1614=VERTEX_POINT('',#5805);
#1615=VERTEX_POINT('',#5807);
#1616=VERTEX_POINT('',#5824);
#1617=VERTEX_POINT('',#5837);
#1618=VERTEX_POINT('',#5839);
#1619=VERTEX_POINT('',#5841);
#1620=VERTEX_POINT('',#5843);
#1621=VERTEX_POINT('',#5860);
#1622=VERTEX_POINT('',#5862);
#1623=VERTEX_POINT('',#5881);
#1624=VERTEX_POINT('',#5883);
#1625=VERTEX_POINT('',#5885);
#1626=VERTEX_POINT('',#5887);
#1627=VERTEX_POINT('',#5904);
#1628=VERTEX_POINT('',#5906);
#1629=VERTEX_POINT('',#5925);
#1630=VERTEX_POINT('',#5927);
#1631=VERTEX_POINT('',#5929);
#1632=VERTEX_POINT('',#5938);
#1633=VERTEX_POINT('',#5940);
#1634=VERTEX_POINT('',#5957);
#1635=VERTEX_POINT('',#5972);
#1636=VERTEX_POINT('',#5974);
#1637=VERTEX_POINT('',#5976);
#1638=VERTEX_POINT('',#5993);
#1639=VERTEX_POINT('',#5995);
#1640=VERTEX_POINT('',#6012);
#1641=VERTEX_POINT('',#6019);
#1642=VERTEX_POINT('',#6021);
#1643=VERTEX_POINT('',#6023);
#1644=VERTEX_POINT('',#6036);
#1645=VERTEX_POINT('',#6038);
#1646=VERTEX_POINT('',#6055);
#1647=VERTEX_POINT('',#6066);
#1648=VERTEX_POINT('',#6068);
#1649=VERTEX_POINT('',#6070);
#1650=VERTEX_POINT('',#6072);
#1651=VERTEX_POINT('',#6089);
#1652=VERTEX_POINT('',#6091);
#1653=VERTEX_POINT('',#6110);
#1654=VERTEX_POINT('',#6112);
#1655=VERTEX_POINT('',#6114);
#1656=VERTEX_POINT('',#6116);
#1657=VERTEX_POINT('',#6133);
#1658=VERTEX_POINT('',#6135);
#1659=VERTEX_POINT('',#6154);
#1660=VERTEX_POINT('',#6156);
#1661=VERTEX_POINT('',#6158);
#1662=VERTEX_POINT('',#6173);
#1663=VERTEX_POINT('',#6175);
#1664=VERTEX_POINT('',#6192);
#1665=VERTEX_POINT('',#6201);
#1666=VERTEX_POINT('',#6203);
#1667=VERTEX_POINT('',#6205);
#1668=VERTEX_POINT('',#6210);
#1669=VERTEX_POINT('',#6212);
#1670=VERTEX_POINT('',#6229);
#1671=VERTEX_POINT('',#6258);
#1672=VERTEX_POINT('',#6281);
#1673=VERTEX_POINT('',#6284);
#1674=VERTEX_POINT('',#6288);
#1675=VERTEX_POINT('',#6294);
#1676=VERTEX_POINT('',#6295);
#1677=VERTEX_POINT('',#6312);
#1678=VERTEX_POINT('',#6314);
#1679=VERTEX_POINT('',#6323);
#1680=VERTEX_POINT('',#6326);
#1681=VERTEX_POINT('',#6341);
#1682=VERTEX_POINT('',#6342);
#1683=VERTEX_POINT('',#6359);
#1684=VERTEX_POINT('',#6361);
#1685=VERTEX_POINT('',#6378);
#1686=VERTEX_POINT('',#6380);
#1687=VERTEX_POINT('',#6385);
#1688=VERTEX_POINT('',#6386);
#1689=VERTEX_POINT('',#6403);
#1690=VERTEX_POINT('',#6405);
#1691=VERTEX_POINT('',#6408);
#1692=VERTEX_POINT('',#6410);
#1693=VERTEX_POINT('',#6429);
#1694=VERTEX_POINT('',#6430);
#1695=VERTEX_POINT('',#6445);
#1696=VERTEX_POINT('',#6447);
#1697=VERTEX_POINT('',#6464);
#1698=VERTEX_POINT('',#6472);
#1699=VERTEX_POINT('',#6476);
#1700=VERTEX_POINT('',#6477);
#1701=VERTEX_POINT('',#6482);
#1702=VERTEX_POINT('',#6484);
#1703=VERTEX_POINT('',#6501);
#1704=VERTEX_POINT('',#6519);
#1705=VERTEX_POINT('',#6523);
#1706=VERTEX_POINT('',#6524);
#1707=VERTEX_POINT('',#6535);
#1708=VERTEX_POINT('',#6537);
#1709=VERTEX_POINT('',#6554);
#1710=VERTEX_POINT('',#6566);
#1711=VERTEX_POINT('',#6570);
#1712=VERTEX_POINT('',#6571);
#1713=VERTEX_POINT('',#6588);
#1714=VERTEX_POINT('',#6590);
#1715=VERTEX_POINT('',#6607);
#1716=VERTEX_POINT('',#6609);
#1717=VERTEX_POINT('',#6614);
#1718=VERTEX_POINT('',#6615);
#1719=VERTEX_POINT('',#6632);
#1720=VERTEX_POINT('',#6634);
#1721=VERTEX_POINT('',#6651);
#1722=VERTEX_POINT('',#6653);
#1723=VERTEX_POINT('',#6658);
#1724=VERTEX_POINT('',#6659);
#1725=VERTEX_POINT('',#6676);
#1726=VERTEX_POINT('',#6678);
#1727=VERTEX_POINT('',#6691);
#1728=VERTEX_POINT('',#6694);
#1729=VERTEX_POINT('',#6705);
#1730=VERTEX_POINT('',#6706);
#1731=VERTEX_POINT('',#6723);
#1732=VERTEX_POINT('',#6725);
#1733=VERTEX_POINT('',#6730);
#1734=VERTEX_POINT('',#6733);
#1735=VERTEX_POINT('',#6762);
#1736=VERTEX_POINT('',#6785);
#1737=VERTEX_POINT('',#6787);
#1738=VERTEX_POINT('',#6790);
#1739=VERTEX_POINT('',#6798);
#1740=VERTEX_POINT('',#6799);
#1741=VERTEX_POINT('',#6802);
#1742=VERTEX_POINT('',#6803);
#1743=VERTEX_POINT('',#6806);
#1744=VERTEX_POINT('',#6807);
#1745=VERTEX_POINT('',#6810);
#1746=VERTEX_POINT('',#6811);
#1747=VERTEX_POINT('',#6814);
#1748=VERTEX_POINT('',#6815);
#1749=VERTEX_POINT('',#6818);
#1750=VERTEX_POINT('',#6819);
#1751=VERTEX_POINT('',#6822);
#1752=VERTEX_POINT('',#6823);
#1753=VERTEX_POINT('',#6826);
#1754=VERTEX_POINT('',#6827);
#1755=VERTEX_POINT('',#6830);
#1756=VERTEX_POINT('',#6831);
#1757=VERTEX_POINT('',#6834);
#1758=VERTEX_POINT('',#6835);
#1759=VERTEX_POINT('',#6842);
#1760=VERTEX_POINT('',#6844);
#1761=VERTEX_POINT('',#6848);
#1762=VERTEX_POINT('',#6850);
#1763=VERTEX_POINT('',#6857);
#1764=VERTEX_POINT('',#6858);
#1765=VERTEX_POINT('',#6862);
#1766=VERTEX_POINT('',#6866);
#1767=VERTEX_POINT('',#6869);
#1768=VERTEX_POINT('',#6873);
#1769=VERTEX_POINT('',#6877);
#1770=VERTEX_POINT('',#6885);
#1771=VERTEX_POINT('',#6887);
#1772=VERTEX_POINT('',#6889);
#1773=VERTEX_POINT('',#6893);
#1774=VERTEX_POINT('',#6897);
#1775=VERTEX_POINT('',#6901);
#1776=VERTEX_POINT('',#6905);
#1777=VERTEX_POINT('',#6920);
#1778=VERTEX_POINT('',#6922);
#1779=VERTEX_POINT('',#6940);
#1780=VERTEX_POINT('',#6942);
#1781=VERTEX_POINT('',#6946);
#1782=VERTEX_POINT('',#6947);
#1783=VERTEX_POINT('',#6949);
#1784=VERTEX_POINT('',#6951);
#1785=VERTEX_POINT('',#6955);
#1786=VERTEX_POINT('',#6956);
#1787=VERTEX_POINT('',#6958);
#1788=VERTEX_POINT('',#6960);
#1789=VERTEX_POINT('',#6964);
#1790=VERTEX_POINT('',#6966);
#1791=VERTEX_POINT('',#6968);
#1792=VERTEX_POINT('',#6970);
#1793=VERTEX_POINT('',#6972);
#1794=VERTEX_POINT('',#6974);
#1795=VERTEX_POINT('',#6976);
#1796=VERTEX_POINT('',#6978);
#1797=VERTEX_POINT('',#6982);
#1798=VERTEX_POINT('',#6986);
#1799=VERTEX_POINT('',#6990);
#1800=VERTEX_POINT('',#6992);
#1801=VERTEX_POINT('',#6994);
#1802=VERTEX_POINT('',#6996);
#1803=VERTEX_POINT('',#6998);
#1804=VERTEX_POINT('',#7000);
#1805=VERTEX_POINT('',#7002);
#1806=VERTEX_POINT('',#7004);
#1807=VERTEX_POINT('',#7008);
#1808=VERTEX_POINT('',#7012);
#1809=VERTEX_POINT('',#7016);
#1810=VERTEX_POINT('',#7023);
#1811=VERTEX_POINT('',#7025);
#1812=VERTEX_POINT('',#7030);
#1813=VERTEX_POINT('',#7045);
#1814=VERTEX_POINT('',#7047);
#1815=VERTEX_POINT('',#7051);
#1816=VERTEX_POINT('',#7053);
#1817=VERTEX_POINT('',#7060);
#1818=VERTEX_POINT('',#7062);
#1819=VERTEX_POINT('',#7067);
#1820=VERTEX_POINT('',#7069);
#1821=VERTEX_POINT('',#7072);
#1822=VERTEX_POINT('',#7077);
#1823=VERTEX_POINT('',#7083);
#1824=VERTEX_POINT('',#7085);
#1825=VERTEX_POINT('',#7089);
#1826=VERTEX_POINT('',#7091);
#1827=VERTEX_POINT('',#7098);
#1828=VERTEX_POINT('',#7100);
#1829=VERTEX_POINT('',#7104);
#1830=VERTEX_POINT('',#7106);
#1831=VERTEX_POINT('',#7113);
#1832=VERTEX_POINT('',#7114);
#1833=VERTEX_POINT('',#7116);
#1834=VERTEX_POINT('',#7118);
#1835=VERTEX_POINT('',#7122);
#1836=VERTEX_POINT('',#7124);
#1837=VERTEX_POINT('',#7128);
#1838=VERTEX_POINT('',#7130);
#1839=VERTEX_POINT('',#7134);
#1840=VERTEX_POINT('',#7136);
#1841=VERTEX_POINT('',#7140);
#1842=VERTEX_POINT('',#7142);
#1843=VERTEX_POINT('',#7151);
#1844=VERTEX_POINT('',#7154);
#1845=VERTEX_POINT('',#7157);
#1846=VERTEX_POINT('',#7161);
#1847=VERTEX_POINT('',#7165);
#1848=VERTEX_POINT('',#7169);
#1849=VERTEX_POINT('',#7172);
#1850=VERTEX_POINT('',#7187);
#1851=VERTEX_POINT('',#7189);
#1852=VERTEX_POINT('',#7193);
#1853=VERTEX_POINT('',#7196);
#1854=VERTEX_POINT('',#7198);
#1855=VERTEX_POINT('',#7202);
#1856=VERTEX_POINT('',#7207);
#1857=VERTEX_POINT('',#7209);
#1858=VERTEX_POINT('',#7217);
#1859=VERTEX_POINT('',#7218);
#1860=VERTEX_POINT('',#7221);
#1861=VERTEX_POINT('',#7223);
#1862=VERTEX_POINT('',#7227);
#1863=VERTEX_POINT('',#7231);
#1864=VERTEX_POINT('',#7233);
#1865=VERTEX_POINT('',#7237);
#1866=VERTEX_POINT('',#7242);
#1867=VERTEX_POINT('',#7246);
#1868=VERTEX_POINT('',#7252);
#1869=VERTEX_POINT('',#7253);
#1870=VERTEX_POINT('',#7256);
#1871=VERTEX_POINT('',#7258);
#1872=VERTEX_POINT('',#7262);
#1873=VERTEX_POINT('',#7266);
#1874=VERTEX_POINT('',#7268);
#1875=VERTEX_POINT('',#7271);
#1876=VERTEX_POINT('',#7275);
#1877=VERTEX_POINT('',#7279);
#1878=VERTEX_POINT('',#7287);
#1879=VERTEX_POINT('',#7288);
#1880=VERTEX_POINT('',#7291);
#1881=VERTEX_POINT('',#7292);
#1882=VERTEX_POINT('',#7295);
#1883=VERTEX_POINT('',#7296);
#1884=VERTEX_POINT('',#7299);
#1885=VERTEX_POINT('',#7300);
#1886=VERTEX_POINT('',#7303);
#1887=VERTEX_POINT('',#7304);
#1888=VERTEX_POINT('',#7307);
#1889=VERTEX_POINT('',#7308);
#1890=VERTEX_POINT('',#7311);
#1891=VERTEX_POINT('',#7312);
#1892=VERTEX_POINT('',#7316);
#1893=VERTEX_POINT('',#7317);
#1894=VERTEX_POINT('',#7340);
#1895=VERTEX_POINT('',#7342);
#1896=VERTEX_POINT('',#7367);
#1897=VERTEX_POINT('',#7369);
#1898=VERTEX_POINT('',#7392);
#1899=VERTEX_POINT('',#7394);
#1900=VERTEX_POINT('',#7417);
#1901=VERTEX_POINT('',#7419);
#1902=VERTEX_POINT('',#7422);
#1903=VERTEX_POINT('',#7424);
#1904=VERTEX_POINT('',#7447);
#1905=VERTEX_POINT('',#7449);
#1906=VERTEX_POINT('',#7472);
#1907=VERTEX_POINT('',#7474);
#1908=VERTEX_POINT('',#7497);
#1909=VERTEX_POINT('',#7499);
#1910=VERTEX_POINT('',#7524);
#1911=VERTEX_POINT('',#7528);
#1912=VERTEX_POINT('',#7553);
#1913=VERTEX_POINT('',#7557);
#1914=VERTEX_POINT('',#7582);
#1915=VERTEX_POINT('',#7584);
#1916=VERTEX_POINT('',#7588);
#1917=VERTEX_POINT('',#7613);
#1918=VERTEX_POINT('',#7617);
#1919=VERTEX_POINT('',#7642);
#1920=VERTEX_POINT('',#7646);
#1921=VERTEX_POINT('',#7671);
#1922=VERTEX_POINT('',#7674);
#1923=VERTEX_POINT('',#7676);
#1924=VERTEX_POINT('',#7708);
#1925=VERTEX_POINT('',#7710);
#1926=VERTEX_POINT('',#7713);
#1927=VERTEX_POINT('',#7717);
#1928=VERTEX_POINT('',#7722);
#1929=VERTEX_POINT('',#7724);
#1930=VERTEX_POINT('',#7727);
#1931=VERTEX_POINT('',#7731);
#1932=VERTEX_POINT('',#7742);
#1933=VERTEX_POINT('',#7744);
#1934=VERTEX_POINT('',#7748);
#1935=VERTEX_POINT('',#7750);
#1936=EDGE_CURVE('',#1585,#1585,#1321,.T.);
#1937=EDGE_CURVE('',#1585,#1586,#1011,.T.);
#1938=EDGE_CURVE('',#1586,#1586,#1322,.T.);
#1939=EDGE_CURVE('',#1587,#1587,#1323,.T.);
#1940=EDGE_CURVE('',#1587,#1588,#1012,.T.);
#1941=EDGE_CURVE('',#1588,#1588,#1324,.T.);
#1942=EDGE_CURVE('',#1589,#1589,#1325,.T.);
#1943=EDGE_CURVE('',#1589,#1590,#1013,.T.);
#1944=EDGE_CURVE('',#1590,#1590,#1326,.T.);
#1945=EDGE_CURVE('',#1591,#1591,#1327,.T.);
#1946=EDGE_CURVE('',#1591,#1592,#1014,.T.);
#1947=EDGE_CURVE('',#1592,#1592,#1328,.T.);
#1948=EDGE_CURVE('',#1593,#1593,#1329,.T.);
#1949=EDGE_CURVE('',#1593,#1594,#1015,.T.);
#1950=EDGE_CURVE('',#1594,#1594,#1330,.T.);
#1951=EDGE_CURVE('',#1595,#1596,#1016,.T.);
#1952=EDGE_CURVE('',#1596,#1597,#1017,.T.);
#1953=EDGE_CURVE('',#1598,#1597,#1018,.T.);
#1954=EDGE_CURVE('',#1595,#1598,#1019,.T.);
#1955=EDGE_CURVE('',#1599,#1595,#1020,.T.);
#1956=EDGE_CURVE('',#1600,#1598,#1021,.T.);
#1957=EDGE_CURVE('',#1599,#1600,#1022,.T.);
#1958=EDGE_CURVE('',#1601,#1599,#1023,.T.);
#1959=EDGE_CURVE('',#1602,#1600,#1024,.T.);
#1960=EDGE_CURVE('',#1601,#1602,#1025,.T.);
#1961=EDGE_CURVE('',#1596,#1601,#1026,.T.);
#1962=EDGE_CURVE('',#1597,#1602,#1027,.T.);
#1963=EDGE_CURVE('',#1603,#1603,#1331,.T.);
#1964=EDGE_CURVE('',#1603,#1604,#1028,.T.);
#1965=EDGE_CURVE('',#1604,#1604,#1332,.T.);
#1966=EDGE_CURVE('',#1605,#1605,#1333,.T.);
#1967=EDGE_CURVE('',#1606,#1606,#1334,.T.);
#1968=EDGE_CURVE('',#1607,#1607,#1335,.T.);
#1969=EDGE_CURVE('',#1607,#1605,#1029,.T.);
#1970=EDGE_CURVE('',#1608,#1608,#1336,.T.);
#1971=EDGE_CURVE('',#1609,#1609,#1337,.T.);
#1972=EDGE_CURVE('',#1606,#1608,#1030,.T.);
#1973=EDGE_CURVE('',#1609,#1610,#1031,.T.);
#1974=EDGE_CURVE('',#1610,#1610,#1338,.T.);
#1975=EDGE_CURVE('',#1611,#1611,#1339,.T.);
#1976=EDGE_CURVE('',#1611,#1612,#1032,.T.);
#1977=EDGE_CURVE('',#1613,#1612,#192,.T.);
#1978=EDGE_CURVE('',#1614,#1613,#1340,.T.);
#1979=EDGE_CURVE('',#1615,#1614,#193,.T.);
#1980=EDGE_CURVE('',#1616,#1615,#1341,.T.);
#1981=EDGE_CURVE('',#1612,#1616,#194,.T.);
#1982=EDGE_CURVE('',#1617,#1617,#1342,.T.);
#1983=EDGE_CURVE('',#1617,#1618,#1033,.T.);
#1984=EDGE_CURVE('',#1619,#1618,#1343,.T.);
#1985=EDGE_CURVE('',#1620,#1619,#195,.T.);
#1986=EDGE_CURVE('',#1621,#1620,#1344,.T.);
#1987=EDGE_CURVE('',#1622,#1621,#196,.T.);
#1988=EDGE_CURVE('',#1618,#1622,#1345,.T.);
#1989=EDGE_CURVE('',#1623,#1623,#1346,.T.);
#1990=EDGE_CURVE('',#1623,#1624,#1034,.T.);
#1991=EDGE_CURVE('',#1625,#1624,#1347,.T.);
#1992=EDGE_CURVE('',#1626,#1625,#197,.T.);
#1993=EDGE_CURVE('',#1627,#1626,#1348,.T.);
#1994=EDGE_CURVE('',#1628,#1627,#198,.T.);
#1995=EDGE_CURVE('',#1624,#1628,#1349,.T.);
#1996=EDGE_CURVE('',#1629,#1629,#1350,.T.);
#1997=EDGE_CURVE('',#1629,#1630,#1035,.T.);
#1998=EDGE_CURVE('',#1631,#1630,#199,.T.);
#1999=EDGE_CURVE('',#1632,#1631,#1351,.T.);
#2000=EDGE_CURVE('',#1633,#1632,#200,.T.);
#2001=EDGE_CURVE('',#1634,#1633,#1352,.T.);
#2002=EDGE_CURVE('',#1630,#1634,#201,.T.);
#2003=EDGE_CURVE('',#1635,#1635,#1353,.T.);
#2004=EDGE_CURVE('',#1635,#1636,#1036,.T.);
#2005=EDGE_CURVE('',#1637,#1636,#202,.T.);
#2006=EDGE_CURVE('',#1638,#1637,#1354,.T.);
#2007=EDGE_CURVE('',#1639,#1638,#203,.T.);
#2008=EDGE_CURVE('',#1640,#1639,#1355,.T.);
#2009=EDGE_CURVE('',#1636,#1640,#204,.T.);
#2010=EDGE_CURVE('',#1641,#1641,#1356,.T.);
#2011=EDGE_CURVE('',#1641,#1642,#1037,.T.);
#2012=EDGE_CURVE('',#1643,#1642,#205,.T.);
#2013=EDGE_CURVE('',#1644,#1643,#1357,.T.);
#2014=EDGE_CURVE('',#1645,#1644,#206,.T.);
#2015=EDGE_CURVE('',#1646,#1645,#1358,.T.);
#2016=EDGE_CURVE('',#1642,#1646,#207,.T.);
#2017=EDGE_CURVE('',#1647,#1647,#1359,.T.);
#2018=EDGE_CURVE('',#1647,#1648,#1038,.T.);
#2019=EDGE_CURVE('',#1649,#1648,#1360,.T.);
#2020=EDGE_CURVE('',#1650,#1649,#208,.T.);
#2021=EDGE_CURVE('',#1651,#1650,#1361,.T.);
#2022=EDGE_CURVE('',#1652,#1651,#209,.T.);
#2023=EDGE_CURVE('',#1648,#1652,#1362,.T.);
#2024=EDGE_CURVE('',#1653,#1653,#1363,.T.);
#2025=EDGE_CURVE('',#1653,#1654,#1039,.T.);
#2026=EDGE_CURVE('',#1655,#1654,#1364,.T.);
#2027=EDGE_CURVE('',#1656,#1655,#210,.T.);
#2028=EDGE_CURVE('',#1657,#1656,#1365,.T.);
#2029=EDGE_CURVE('',#1658,#1657,#211,.T.);
#2030=EDGE_CURVE('',#1654,#1658,#1366,.T.);
#2031=EDGE_CURVE('',#1659,#1659,#1367,.T.);
#2032=EDGE_CURVE('',#1659,#1660,#1040,.T.);
#2033=EDGE_CURVE('',#1661,#1660,#212,.T.);
#2034=EDGE_CURVE('',#1662,#1661,#1368,.T.);
#2035=EDGE_CURVE('',#1663,#1662,#213,.T.);
#2036=EDGE_CURVE('',#1664,#1663,#1369,.T.);
#2037=EDGE_CURVE('',#1660,#1664,#214,.T.);
#2038=EDGE_CURVE('',#1665,#1665,#1370,.T.);
#2039=EDGE_CURVE('',#1665,#1666,#1041,.T.);
#2040=EDGE_CURVE('',#1667,#1666,#215,.T.);
#2041=EDGE_CURVE('',#1668,#1667,#1371,.T.);
#2042=EDGE_CURVE('',#1669,#1668,#216,.T.);
#2043=EDGE_CURVE('',#1670,#1669,#1372,.T.);
#2044=EDGE_CURVE('',#1666,#1670,#217,.T.);
#2045=EDGE_CURVE('',#1613,#1662,#1373,.T.);
#2046=EDGE_CURVE('',#1661,#1621,#1374,.T.);
#2047=EDGE_CURVE('',#1620,#1657,#1375,.T.);
#2048=EDGE_CURVE('',#1656,#1651,#1376,.T.);
#2049=EDGE_CURVE('',#1650,#1634,#1377,.T.);
#2050=EDGE_CURVE('',#1633,#1646,#1378,.T.);
#2051=EDGE_CURVE('',#1645,#1640,#1379,.T.);
#2052=EDGE_CURVE('',#1639,#1625,#1380,.T.);
#2053=EDGE_CURVE('',#1628,#1668,#1381,.T.);
#2054=EDGE_CURVE('',#1667,#1614,#1382,.T.);
#2055=EDGE_CURVE('',#1671,#1671,#1383,.T.);
#2056=EDGE_CURVE('',#1652,#1655,#1384,.T.);
#2057=EDGE_CURVE('',#1637,#1644,#1385,.T.);
#2058=EDGE_CURVE('',#1631,#1649,#1386,.T.);
#2059=EDGE_CURVE('',#1643,#1632,#1387,.T.);
#2060=EDGE_CURVE('',#1626,#1638,#1388,.T.);
#2061=EDGE_CURVE('',#1669,#1627,#1389,.T.);
#2062=EDGE_CURVE('',#1622,#1664,#1390,.T.);
#2063=EDGE_CURVE('',#1658,#1619,#1391,.T.);
#2064=EDGE_CURVE('',#1615,#1670,#1392,.T.);
#2065=EDGE_CURVE('',#1663,#1616,#1393,.T.);
#2066=EDGE_CURVE('',#1672,#1672,#1394,.T.);
#2067=EDGE_CURVE('',#1673,#1673,#1395,.T.);
#2068=EDGE_CURVE('',#1673,#1672,#1042,.T.);
#2069=EDGE_CURVE('',#1674,#1674,#1396,.T.);
#2070=EDGE_CURVE('',#1674,#1671,#1043,.T.);
#2071=EDGE_CURVE('',#1675,#1676,#218,.T.);
#2072=EDGE_CURVE('',#1677,#1675,#1397,.T.);
#2073=EDGE_CURVE('',#1678,#1677,#219,.T.);
#2074=EDGE_CURVE('',#1678,#1679,#1044,.T.);
#2075=EDGE_CURVE('',#1679,#1679,#1398,.T.);
#2076=EDGE_CURVE('',#1680,#1678,#220,.T.);
#2077=EDGE_CURVE('',#1676,#1680,#1399,.T.);
#2078=EDGE_CURVE('',#1681,#1682,#221,.T.);
#2079=EDGE_CURVE('',#1683,#1681,#1400,.T.);
#2080=EDGE_CURVE('',#1684,#1683,#222,.T.);
#2081=EDGE_CURVE('',#1685,#1684,#1401,.T.);
#2082=EDGE_CURVE('',#1685,#1686,#1045,.T.);
#2083=EDGE_CURVE('',#1686,#1686,#1402,.T.);
#2084=EDGE_CURVE('',#1682,#1685,#1403,.T.);
#2085=EDGE_CURVE('',#1687,#1688,#223,.T.);
#2086=EDGE_CURVE('',#1689,#1687,#1404,.T.);
#2087=EDGE_CURVE('',#1689,#1690,#1046,.T.);
#2088=EDGE_CURVE('',#1690,#1690,#1405,.T.);
#2089=EDGE_CURVE('',#1691,#1689,#1406,.T.);
#2090=EDGE_CURVE('',#1692,#1691,#224,.T.);
#2091=EDGE_CURVE('',#1688,#1692,#1407,.T.);
#2092=EDGE_CURVE('',#1693,#1694,#225,.T.);
#2093=EDGE_CURVE('',#1695,#1693,#1408,.T.);
#2094=EDGE_CURVE('',#1696,#1695,#226,.T.);
#2095=EDGE_CURVE('',#1697,#1696,#1409,.T.);
#2096=EDGE_CURVE('',#1694,#1697,#227,.T.);
#2097=EDGE_CURVE('',#1694,#1698,#1047,.T.);
#2098=EDGE_CURVE('',#1698,#1698,#1410,.T.);
#2099=EDGE_CURVE('',#1699,#1700,#228,.T.);
#2100=EDGE_CURVE('',#1701,#1699,#1411,.T.);
#2101=EDGE_CURVE('',#1702,#1701,#229,.T.);
#2102=EDGE_CURVE('',#1703,#1702,#1412,.T.);
#2103=EDGE_CURVE('',#1700,#1703,#230,.T.);
#2104=EDGE_CURVE('',#1700,#1704,#1048,.T.);
#2105=EDGE_CURVE('',#1704,#1704,#1413,.T.);
#2106=EDGE_CURVE('',#1705,#1706,#231,.T.);
#2107=EDGE_CURVE('',#1707,#1705,#1414,.T.);
#2108=EDGE_CURVE('',#1708,#1707,#232,.T.);
#2109=EDGE_CURVE('',#1709,#1708,#1415,.T.);
#2110=EDGE_CURVE('',#1706,#1709,#233,.T.);
#2111=EDGE_CURVE('',#1706,#1710,#1049,.T.);
#2112=EDGE_CURVE('',#1710,#1710,#1416,.T.);
#2113=EDGE_CURVE('',#1711,#1712,#234,.T.);
#2114=EDGE_CURVE('',#1713,#1711,#1417,.T.);
#2115=EDGE_CURVE('',#1714,#1713,#235,.T.);
#2116=EDGE_CURVE('',#1715,#1714,#1418,.T.);
#2117=EDGE_CURVE('',#1715,#1716,#1050,.T.);
#2118=EDGE_CURVE('',#1716,#1716,#1419,.T.);
#2119=EDGE_CURVE('',#1712,#1715,#1420,.T.);
#2120=EDGE_CURVE('',#1717,#1718,#236,.T.);
#2121=EDGE_CURVE('',#1719,#1717,#1421,.T.);
#2122=EDGE_CURVE('',#1720,#1719,#237,.T.);
#2123=EDGE_CURVE('',#1721,#1720,#1422,.T.);
#2124=EDGE_CURVE('',#1721,#1722,#1051,.T.);
#2125=EDGE_CURVE('',#1722,#1722,#1423,.T.);
#2126=EDGE_CURVE('',#1718,#1721,#1424,.T.);
#2127=EDGE_CURVE('',#1723,#1724,#238,.T.);
#2128=EDGE_CURVE('',#1725,#1723,#1425,.T.);
#2129=EDGE_CURVE('',#1726,#1725,#239,.T.);
#2130=EDGE_CURVE('',#1726,#1727,#1052,.T.);
#2131=EDGE_CURVE('',#1727,#1727,#1426,.T.);
#2132=EDGE_CURVE('',#1728,#1726,#240,.T.);
#2133=EDGE_CURVE('',#1724,#1728,#1427,.T.);
#2134=EDGE_CURVE('',#1729,#1730,#241,.T.);
#2135=EDGE_CURVE('',#1731,#1729,#1428,.T.);
#2136=EDGE_CURVE('',#1732,#1731,#242,.T.);
#2137=EDGE_CURVE('',#1732,#1733,#1053,.T.);
#2138=EDGE_CURVE('',#1733,#1733,#1429,.T.);
#2139=EDGE_CURVE('',#1734,#1732,#243,.T.);
#2140=EDGE_CURVE('',#1730,#1734,#1430,.T.);
#2141=EDGE_CURVE('',#1675,#1731,#1431,.T.);
#2142=EDGE_CURVE('',#1729,#1691,#1432,.T.);
#2143=EDGE_CURVE('',#1687,#1701,#1433,.T.);
#2144=EDGE_CURVE('',#1699,#1707,#1434,.T.);
#2145=EDGE_CURVE('',#1705,#1695,#1435,.T.);
#2146=EDGE_CURVE('',#1693,#1713,#1436,.T.);
#2147=EDGE_CURVE('',#1711,#1719,#1437,.T.);
#2148=EDGE_CURVE('',#1717,#1683,#1438,.T.);
#2149=EDGE_CURVE('',#1681,#1725,#1439,.T.);
#2150=EDGE_CURVE('',#1723,#1677,#1440,.T.);
#2151=EDGE_CURVE('',#1735,#1735,#1441,.T.);
#2152=EDGE_CURVE('',#1720,#1712,#1442,.T.);
#2153=EDGE_CURVE('',#1708,#1703,#1443,.T.);
#2154=EDGE_CURVE('',#1714,#1697,#1444,.T.);
#2155=EDGE_CURVE('',#1696,#1709,#1445,.T.);
#2156=EDGE_CURVE('',#1702,#1688,#1446,.T.);
#2157=EDGE_CURVE('',#1692,#1730,#1447,.T.);
#2158=EDGE_CURVE('',#1728,#1682,#1448,.T.);
#2159=EDGE_CURVE('',#1684,#1718,#1449,.T.);
#2160=EDGE_CURVE('',#1734,#1676,#1450,.T.);
#2161=EDGE_CURVE('',#1680,#1724,#1451,.T.);
#2162=EDGE_CURVE('',#1736,#1736,#1452,.T.);
#2163=EDGE_CURVE('',#1737,#1737,#1453,.T.);
#2164=EDGE_CURVE('',#1738,#1738,#1454,.T.);
#2165=EDGE_CURVE('',#1738,#1736,#1054,.T.);
#2166=EDGE_CURVE('',#1735,#1737,#1055,.T.);
#2167=EDGE_CURVE('',#1739,#1740,#1455,.T.);
#2168=EDGE_CURVE('',#1741,#1742,#1456,.T.);
#2169=EDGE_CURVE('',#1743,#1744,#1457,.T.);
#2170=EDGE_CURVE('',#1745,#1746,#1458,.T.);
#2171=EDGE_CURVE('',#1747,#1748,#1459,.T.);
#2172=EDGE_CURVE('',#1749,#1750,#1460,.T.);
#2173=EDGE_CURVE('',#1751,#1752,#1461,.T.);
#2174=EDGE_CURVE('',#1753,#1754,#1462,.T.);
#2175=EDGE_CURVE('',#1755,#1756,#1463,.T.);
#2176=EDGE_CURVE('',#1757,#1758,#1464,.T.);
#2177=EDGE_CURVE('',#1759,#1759,#1465,.T.);
#2178=EDGE_CURVE('',#1759,#1760,#1056,.T.);
#2179=EDGE_CURVE('',#1760,#1760,#1466,.T.);
#2180=EDGE_CURVE('',#1761,#1761,#1467,.T.);
#2181=EDGE_CURVE('',#1761,#1762,#1057,.T.);
#2182=EDGE_CURVE('',#1762,#1762,#1468,.T.);
#2183=EDGE_CURVE('',#1763,#1764,#13,.T.);
#2184=EDGE_CURVE('',#1765,#1763,#14,.T.);
#2185=EDGE_CURVE('',#1765,#1766,#1058,.T.);
#2186=EDGE_CURVE('',#1766,#1766,#1469,.T.);
#2187=EDGE_CURVE('',#1767,#1765,#15,.T.);
#2188=EDGE_CURVE('',#1768,#1767,#16,.T.);
#2189=EDGE_CURVE('',#1769,#1768,#17,.T.);
#2190=EDGE_CURVE('',#1764,#1769,#18,.T.);
#2191=EDGE_CURVE('',#1770,#1770,#1470,.T.);
#2192=EDGE_CURVE('',#1770,#1771,#1059,.T.);
#2193=EDGE_CURVE('',#1772,#1771,#19,.T.);
#2194=EDGE_CURVE('',#1773,#1772,#20,.T.);
#2195=EDGE_CURVE('',#1774,#1773,#21,.T.);
#2196=EDGE_CURVE('',#1775,#1774,#22,.T.);
#2197=EDGE_CURVE('',#1776,#1775,#23,.T.);
#2198=EDGE_CURVE('',#1771,#1776,#24,.T.);
#2199=EDGE_CURVE('',#1767,#1776,#1060,.T.);
#2200=EDGE_CURVE('',#1768,#1775,#1061,.T.);
#2201=EDGE_CURVE('',#1765,#1771,#1062,.T.);
#2202=EDGE_CURVE('',#1763,#1772,#1063,.T.);
#2203=EDGE_CURVE('',#1777,#1777,#1471,.F.);
#2204=EDGE_CURVE('',#1777,#1778,#1064,.T.);
#2205=EDGE_CURVE('',#1778,#1778,#1472,.F.);
#2206=EDGE_CURVE('',#1764,#1773,#1065,.T.);
#2207=EDGE_CURVE('',#1769,#1774,#1066,.T.);
#2208=EDGE_CURVE('',#1779,#1779,#1473,.T.);
#2209=EDGE_CURVE('',#1779,#1780,#1067,.T.);
#2210=EDGE_CURVE('',#1780,#1780,#1474,.T.);
#2211=EDGE_CURVE('',#1781,#1782,#1475,.T.);
#2212=EDGE_CURVE('',#1783,#1781,#1068,.T.);
#2213=EDGE_CURVE('',#1784,#1783,#1476,.T.);
#2214=EDGE_CURVE('',#1782,#1784,#1069,.T.);
#2215=EDGE_CURVE('',#1785,#1786,#1070,.T.);
#2216=EDGE_CURVE('',#1787,#1785,#1477,.T.);
#2217=EDGE_CURVE('',#1788,#1787,#1071,.T.);
#2218=EDGE_CURVE('',#1786,#1788,#1478,.T.);
#2219=EDGE_CURVE('',#1785,#1789,#1072,.T.);
#2220=EDGE_CURVE('',#1789,#1790,#1073,.T.);
#2221=EDGE_CURVE('',#1790,#1791,#1074,.T.);
#2222=EDGE_CURVE('',#1791,#1792,#1075,.T.);
#2223=EDGE_CURVE('',#1793,#1792,#1076,.T.);
#2224=EDGE_CURVE('',#1794,#1793,#1077,.T.);
#2225=EDGE_CURVE('',#1794,#1795,#1078,.T.);
#2226=EDGE_CURVE('',#1795,#1796,#1079,.T.);
#2227=EDGE_CURVE('',#1796,#1787,#1080,.T.);
#2228=EDGE_CURVE('',#1797,#1786,#1081,.T.);
#2229=EDGE_CURVE('',#1797,#1789,#1082,.T.);
#2230=EDGE_CURVE('',#1798,#1796,#1083,.T.);
#2231=EDGE_CURVE('',#1788,#1798,#1084,.T.);
#2232=EDGE_CURVE('',#1783,#1799,#1085,.T.);
#2233=EDGE_CURVE('',#1799,#1800,#1086,.T.);
#2234=EDGE_CURVE('',#1800,#1801,#1087,.T.);
#2235=EDGE_CURVE('',#1801,#1802,#1088,.T.);
#2236=EDGE_CURVE('',#1803,#1802,#1089,.T.);
#2237=EDGE_CURVE('',#1804,#1803,#1090,.T.);
#2238=EDGE_CURVE('',#1804,#1805,#1091,.T.);
#2239=EDGE_CURVE('',#1805,#1806,#1092,.T.);
#2240=EDGE_CURVE('',#1806,#1784,#1093,.T.);
#2241=EDGE_CURVE('',#1807,#1781,#1094,.T.);
#2242=EDGE_CURVE('',#1799,#1807,#1095,.T.);
#2243=EDGE_CURVE('',#1790,#1808,#1096,.T.);
#2244=EDGE_CURVE('',#1808,#1797,#1097,.T.);
#2245=EDGE_CURVE('',#1809,#1795,#1098,.T.);
#2246=EDGE_CURVE('',#1798,#1809,#1099,.T.);
#2247=EDGE_CURVE('',#1808,#1809,#1100,.T.);
#2248=EDGE_CURVE('',#1801,#1794,#1101,.T.);
#2249=EDGE_CURVE('',#1800,#1810,#1102,.T.);
#2250=EDGE_CURVE('',#1810,#1811,#1103,.T.);
#2251=EDGE_CURVE('',#1811,#1805,#1104,.T.);
#2252=EDGE_CURVE('',#1791,#1804,#1105,.T.);
#2253=EDGE_CURVE('',#1782,#1812,#1106,.T.);
#2254=EDGE_CURVE('',#1812,#1811,#1107,.T.);
#2255=EDGE_CURVE('',#1810,#1807,#1108,.T.);
#2256=EDGE_CURVE('',#1806,#1812,#1109,.T.);
#2257=EDGE_CURVE('',#1802,#1793,#1110,.T.);
#2258=EDGE_CURVE('',#1792,#1803,#1111,.T.);
#2259=EDGE_CURVE('',#1813,#1813,#1479,.T.);
#2260=EDGE_CURVE('',#1813,#1814,#1112,.T.);
#2261=EDGE_CURVE('',#1814,#1814,#1480,.T.);
#2262=EDGE_CURVE('',#1815,#1815,#1481,.T.);
#2263=EDGE_CURVE('',#1815,#1816,#1113,.T.);
#2264=EDGE_CURVE('',#1816,#1816,#1482,.T.);
#2265=EDGE_CURVE('',#1817,#1817,#1483,.T.);
#2266=EDGE_CURVE('',#1817,#1818,#1114,.T.);
#2267=EDGE_CURVE('',#1818,#1818,#1484,.T.);
#2268=EDGE_CURVE('',#1819,#1819,#1485,.T.);
#2269=EDGE_CURVE('',#1820,#1820,#1486,.T.);
#2270=EDGE_CURVE('',#1819,#1821,#1115,.T.);
#2271=EDGE_CURVE('',#1821,#1821,#1487,.T.);
#2272=EDGE_CURVE('',#1822,#1822,#1488,.T.);
#2273=EDGE_CURVE('',#1822,#1820,#1116,.T.);
#2274=EDGE_CURVE('',#1823,#1823,#1489,.T.);
#2275=EDGE_CURVE('',#1823,#1824,#1117,.T.);
#2276=EDGE_CURVE('',#1824,#1824,#1490,.T.);
#2277=EDGE_CURVE('',#1825,#1825,#1491,.T.);
#2278=EDGE_CURVE('',#1825,#1826,#1118,.T.);
#2279=EDGE_CURVE('',#1826,#1826,#1492,.T.);
#2280=EDGE_CURVE('',#1827,#1827,#1493,.T.);
#2281=EDGE_CURVE('',#1827,#1828,#1119,.T.);
#2282=EDGE_CURVE('',#1828,#1828,#1494,.T.);
#2283=EDGE_CURVE('',#1829,#1829,#1495,.T.);
#2284=EDGE_CURVE('',#1829,#1830,#1120,.T.);
#2285=EDGE_CURVE('',#1830,#1830,#1496,.T.);
#2286=EDGE_CURVE('',#1831,#1832,#1121,.T.);
#2287=EDGE_CURVE('',#1832,#1833,#1122,.T.);
#2288=EDGE_CURVE('',#1833,#1834,#1123,.T.);
#2289=EDGE_CURVE('',#1831,#1834,#1124,.T.);
#2290=EDGE_CURVE('',#1832,#1835,#1125,.T.);
#2291=EDGE_CURVE('',#1835,#1836,#1126,.T.);
#2292=EDGE_CURVE('',#1836,#1833,#1127,.T.);
#2293=EDGE_CURVE('',#1835,#1837,#1128,.T.);
#2294=EDGE_CURVE('',#1837,#1838,#1129,.T.);
#2295=EDGE_CURVE('',#1838,#1836,#1130,.T.);
#2296=EDGE_CURVE('',#1837,#1839,#1131,.T.);
#2297=EDGE_CURVE('',#1839,#1840,#1132,.T.);
#2298=EDGE_CURVE('',#1840,#1838,#1133,.T.);
#2299=EDGE_CURVE('',#1839,#1841,#1134,.T.);
#2300=EDGE_CURVE('',#1841,#1842,#1135,.T.);
#2301=EDGE_CURVE('',#1842,#1840,#1136,.T.);
#2302=EDGE_CURVE('',#1841,#1831,#1137,.T.);
#2303=EDGE_CURVE('',#1834,#1842,#1138,.T.);
#2304=EDGE_CURVE('',#1843,#1843,#1497,.T.);
#2305=EDGE_CURVE('',#1844,#1844,#1498,.T.);
#2306=EDGE_CURVE('',#1845,#1845,#1499,.T.);
#2307=EDGE_CURVE('',#1845,#1844,#1139,.T.);
#2308=EDGE_CURVE('',#1846,#1846,#1500,.T.);
#2309=EDGE_CURVE('',#1846,#1845,#1140,.T.);
#2310=EDGE_CURVE('',#1847,#1847,#1501,.T.);
#2311=EDGE_CURVE('',#1847,#1846,#1141,.T.);
#2312=EDGE_CURVE('',#1848,#1848,#1502,.T.);
#2313=EDGE_CURVE('',#1849,#1849,#1503,.F.);
#2314=EDGE_CURVE('',#1849,#1848,#1142,.T.);
#2315=EDGE_CURVE('',#1843,#1849,#1143,.T.);
#2316=EDGE_CURVE('',#1850,#1850,#1504,.T.);
#2317=EDGE_CURVE('',#1850,#1851,#1144,.T.);
#2318=EDGE_CURVE('',#1851,#1851,#1505,.T.);
#2319=EDGE_CURVE('',#1852,#1852,#1506,.T.);
#2320=EDGE_CURVE('',#1853,#1853,#1507,.T.);
#2321=EDGE_CURVE('',#1853,#1854,#1145,.T.);
#2322=EDGE_CURVE('',#1854,#1854,#1508,.T.);
#2323=EDGE_CURVE('',#1855,#1855,#1509,.T.);
#2324=EDGE_CURVE('',#1855,#1852,#1146,.T.);
#2325=EDGE_CURVE('',#1856,#1856,#1510,.T.);
#2326=EDGE_CURVE('',#1856,#1857,#1147,.T.);
#2327=EDGE_CURVE('',#1857,#1857,#1511,.T.);
#2328=EDGE_CURVE('',#1858,#1859,#1512,.T.);
#2329=EDGE_CURVE('',#1859,#1858,#1513,.T.);
#2330=EDGE_CURVE('',#1859,#1860,#1514,.T.);
#2331=EDGE_CURVE('',#1861,#1860,#1515,.T.);
#2332=EDGE_CURVE('',#1860,#1861,#1516,.T.);
#2333=EDGE_CURVE('',#1861,#1862,#1148,.T.);
#2334=EDGE_CURVE('',#1862,#1862,#1517,.T.);
#2335=EDGE_CURVE('',#1863,#1863,#1518,.T.);
#2336=EDGE_CURVE('',#1863,#1864,#1149,.T.);
#2337=EDGE_CURVE('',#1864,#1864,#1519,.T.);
#2338=EDGE_CURVE('',#1864,#1865,#1150,.T.);
#2339=EDGE_CURVE('',#1865,#1865,#1520,.T.);
#2340=EDGE_CURVE('',#1866,#1866,#1521,.T.);
#2341=EDGE_CURVE('',#1866,#1858,#1151,.T.);
#2342=EDGE_CURVE('',#1867,#1867,#1522,.T.);
#2343=EDGE_CURVE('',#1867,#1863,#1152,.T.);
#2344=EDGE_CURVE('',#1868,#1869,#1523,.T.);
#2345=EDGE_CURVE('',#1869,#1868,#1524,.T.);
#2346=EDGE_CURVE('',#1869,#1870,#1525,.T.);
#2347=EDGE_CURVE('',#1871,#1870,#1526,.T.);
#2348=EDGE_CURVE('',#1870,#1871,#1527,.T.);
#2349=EDGE_CURVE('',#1872,#1872,#1528,.T.);
#2350=EDGE_CURVE('',#1872,#1871,#1153,.T.);
#2351=EDGE_CURVE('',#1873,#1873,#1529,.T.);
#2352=EDGE_CURVE('',#1874,#1874,#1530,.T.);
#2353=EDGE_CURVE('',#1875,#1875,#1531,.T.);
#2354=EDGE_CURVE('',#1875,#1873,#1154,.T.);
#2355=EDGE_CURVE('',#1876,#1876,#1532,.T.);
#2356=EDGE_CURVE('',#1876,#1875,#1155,.T.);
#2357=EDGE_CURVE('',#1877,#1877,#1533,.T.);
#2358=EDGE_CURVE('',#1877,#1876,#1156,.T.);
#2359=EDGE_CURVE('',#1868,#1874,#1157,.T.);
#2360=EDGE_CURVE('',#1878,#1879,#1534,.T.);
#2361=EDGE_CURVE('',#1880,#1881,#1535,.T.);
#2362=EDGE_CURVE('',#1882,#1883,#1536,.T.);
#2363=EDGE_CURVE('',#1884,#1885,#1537,.T.);
#2364=EDGE_CURVE('',#1886,#1887,#1538,.T.);
#2365=EDGE_CURVE('',#1888,#1889,#1539,.T.);
#2366=EDGE_CURVE('',#1890,#1891,#1540,.T.);
#2367=EDGE_CURVE('',#1892,#1893,#244,.T.);
#2368=EDGE_CURVE('',#1894,#1892,#1541,.T.);
#2369=EDGE_CURVE('',#1895,#1894,#245,.T.);
#2370=EDGE_CURVE('',#1893,#1895,#1542,.T.);
#2371=EDGE_CURVE('',#1896,#1894,#1543,.T.);
#2372=EDGE_CURVE('',#1896,#1897,#246,.T.);
#2373=EDGE_CURVE('',#1898,#1897,#1544,.T.);
#2374=EDGE_CURVE('',#1898,#1899,#247,.T.);
#2375=EDGE_CURVE('',#1900,#1899,#1545,.T.);
#2376=EDGE_CURVE('',#1900,#1901,#1158,.T.);
#2377=EDGE_CURVE('',#1901,#1901,#1546,.T.);
#2378=EDGE_CURVE('',#1902,#1900,#1547,.T.);
#2379=EDGE_CURVE('',#1902,#1903,#248,.T.);
#2380=EDGE_CURVE('',#1904,#1903,#1548,.T.);
#2381=EDGE_CURVE('',#1904,#1905,#249,.T.);
#2382=EDGE_CURVE('',#1906,#1905,#1549,.T.);
#2383=EDGE_CURVE('',#1906,#1907,#250,.T.);
#2384=EDGE_CURVE('',#1908,#1907,#1550,.T.);
#2385=EDGE_CURVE('',#1908,#1909,#251,.T.);
#2386=EDGE_CURVE('',#1895,#1909,#1551,.T.);
#2387=EDGE_CURVE('',#1892,#1910,#1552,.T.);
#2388=EDGE_CURVE('',#1910,#1896,#1553,.T.);
#2389=EDGE_CURVE('',#1911,#1910,#252,.T.);
#2390=EDGE_CURVE('',#1897,#1911,#1554,.T.);
#2391=EDGE_CURVE('',#1911,#1912,#1555,.T.);
#2392=EDGE_CURVE('',#1912,#1898,#1556,.T.);
#2393=EDGE_CURVE('',#1913,#1912,#253,.T.);
#2394=EDGE_CURVE('',#1899,#1913,#1557,.T.);
#2395=EDGE_CURVE('',#1913,#1914,#1558,.T.);
#2396=EDGE_CURVE('',#1914,#1915,#1559,.T.);
#2397=EDGE_CURVE('',#1915,#1902,#1560,.T.);
#2398=EDGE_CURVE('',#1916,#1915,#254,.T.);
#2399=EDGE_CURVE('',#1903,#1916,#1561,.T.);
#2400=EDGE_CURVE('',#1916,#1917,#1562,.T.);
#2401=EDGE_CURVE('',#1917,#1904,#1563,.T.);
#2402=EDGE_CURVE('',#1918,#1917,#255,.T.);
#2403=EDGE_CURVE('',#1905,#1918,#1564,.T.);
#2404=EDGE_CURVE('',#1918,#1919,#1565,.T.);
#2405=EDGE_CURVE('',#1919,#1906,#1566,.T.);
#2406=EDGE_CURVE('',#1920,#1919,#256,.T.);
#2407=EDGE_CURVE('',#1907,#1920,#1567,.T.);
#2408=EDGE_CURVE('',#1921,#1921,#1568,.T.);
#2409=EDGE_CURVE('',#1921,#1914,#1159,.T.);
#2410=EDGE_CURVE('',#1922,#1893,#1569,.T.);
#2411=EDGE_CURVE('',#1922,#1923,#257,.T.);
#2412=EDGE_CURVE('',#1920,#1923,#1570,.T.);
#2413=EDGE_CURVE('',#1909,#1922,#1571,.T.);
#2414=EDGE_CURVE('',#1923,#1908,#1572,.T.);
#2415=EDGE_CURVE('',#1924,#1924,#1573,.T.);
#2416=EDGE_CURVE('',#1925,#1925,#1574,.T.);
#2417=EDGE_CURVE('',#1926,#1926,#1575,.T.);
#2418=EDGE_CURVE('',#1926,#1924,#1160,.T.);
#2419=EDGE_CURVE('',#1927,#1927,#1576,.T.);
#2420=EDGE_CURVE('',#1927,#1925,#1161,.T.);
#2421=EDGE_CURVE('',#1928,#1928,#1577,.T.);
#2422=EDGE_CURVE('',#1929,#1929,#1578,.T.);
#2423=EDGE_CURVE('',#1930,#1930,#1579,.T.);
#2424=EDGE_CURVE('',#1930,#1928,#1162,.T.);
#2425=EDGE_CURVE('',#1931,#1931,#1580,.T.);
#2426=EDGE_CURVE('',#1931,#1929,#1163,.T.);
#2427=EDGE_CURVE('',#1932,#1932,#1581,.T.);
#2428=EDGE_CURVE('',#1932,#1933,#1164,.T.);
#2429=EDGE_CURVE('',#1933,#1933,#1582,.T.);
#2430=EDGE_CURVE('',#1934,#1934,#1583,.T.);
#2431=EDGE_CURVE('',#1934,#1935,#1165,.T.);
#2432=EDGE_CURVE('',#1935,#1935,#1584,.T.);
#2433=ORIENTED_EDGE('',*,*,#1936,.F.);
#2434=ORIENTED_EDGE('',*,*,#1937,.T.);
#2435=ORIENTED_EDGE('',*,*,#1938,.F.);
#2436=ORIENTED_EDGE('',*,*,#1937,.F.);
#2437=ORIENTED_EDGE('',*,*,#1939,.F.);
#2438=ORIENTED_EDGE('',*,*,#1940,.T.);
#2439=ORIENTED_EDGE('',*,*,#1941,.F.);
#2440=ORIENTED_EDGE('',*,*,#1940,.F.);
#2441=ORIENTED_EDGE('',*,*,#1942,.F.);
#2442=ORIENTED_EDGE('',*,*,#1943,.T.);
#2443=ORIENTED_EDGE('',*,*,#1944,.F.);
#2444=ORIENTED_EDGE('',*,*,#1943,.F.);
#2445=ORIENTED_EDGE('',*,*,#1945,.F.);
#2446=ORIENTED_EDGE('',*,*,#1946,.T.);
#2447=ORIENTED_EDGE('',*,*,#1947,.F.);
#2448=ORIENTED_EDGE('',*,*,#1946,.F.);
#2449=ORIENTED_EDGE('',*,*,#1948,.F.);
#2450=ORIENTED_EDGE('',*,*,#1949,.T.);
#2451=ORIENTED_EDGE('',*,*,#1950,.F.);
#2452=ORIENTED_EDGE('',*,*,#1949,.F.);
#2453=ORIENTED_EDGE('',*,*,#1951,.T.);
#2454=ORIENTED_EDGE('',*,*,#1952,.T.);
#2455=ORIENTED_EDGE('',*,*,#1953,.F.);
#2456=ORIENTED_EDGE('',*,*,#1954,.F.);
#2457=ORIENTED_EDGE('',*,*,#1955,.T.);
#2458=ORIENTED_EDGE('',*,*,#1954,.T.);
#2459=ORIENTED_EDGE('',*,*,#1956,.F.);
#2460=ORIENTED_EDGE('',*,*,#1957,.F.);
#2461=ORIENTED_EDGE('',*,*,#1958,.T.);
#2462=ORIENTED_EDGE('',*,*,#1957,.T.);
#2463=ORIENTED_EDGE('',*,*,#1959,.F.);
#2464=ORIENTED_EDGE('',*,*,#1960,.F.);
#2465=ORIENTED_EDGE('',*,*,#1961,.T.);
#2466=ORIENTED_EDGE('',*,*,#1960,.T.);
#2467=ORIENTED_EDGE('',*,*,#1962,.F.);
#2468=ORIENTED_EDGE('',*,*,#1952,.F.);
#2469=ORIENTED_EDGE('',*,*,#1962,.T.);
#2470=ORIENTED_EDGE('',*,*,#1959,.T.);
#2471=ORIENTED_EDGE('',*,*,#1956,.T.);
#2472=ORIENTED_EDGE('',*,*,#1953,.T.);
#2473=ORIENTED_EDGE('',*,*,#1938,.T.);
#2474=ORIENTED_EDGE('',*,*,#1941,.T.);
#2475=ORIENTED_EDGE('',*,*,#1944,.T.);
#2476=ORIENTED_EDGE('',*,*,#1947,.T.);
#2477=ORIENTED_EDGE('',*,*,#1950,.T.);
#2478=ORIENTED_EDGE('',*,*,#1961,.F.);
#2479=ORIENTED_EDGE('',*,*,#1951,.F.);
#2480=ORIENTED_EDGE('',*,*,#1955,.F.);
#2481=ORIENTED_EDGE('',*,*,#1958,.F.);
#2482=ORIENTED_EDGE('',*,*,#1936,.T.);
#2483=ORIENTED_EDGE('',*,*,#1939,.T.);
#2484=ORIENTED_EDGE('',*,*,#1942,.T.);
#2485=ORIENTED_EDGE('',*,*,#1945,.T.);
#2486=ORIENTED_EDGE('',*,*,#1948,.T.);
#2487=ORIENTED_EDGE('',*,*,#1963,.F.);
#2488=ORIENTED_EDGE('',*,*,#1964,.T.);
#2489=ORIENTED_EDGE('',*,*,#1965,.T.);
#2490=ORIENTED_EDGE('',*,*,#1964,.F.);
#2491=ORIENTED_EDGE('',*,*,#1965,.F.);
#2492=ORIENTED_EDGE('',*,*,#1966,.F.);
#2493=ORIENTED_EDGE('',*,*,#1967,.T.);
#2494=ORIENTED_EDGE('',*,*,#1968,.F.);
#2495=ORIENTED_EDGE('',*,*,#1969,.T.);
#2496=ORIENTED_EDGE('',*,*,#1966,.T.);
#2497=ORIENTED_EDGE('',*,*,#1969,.F.);
#2498=ORIENTED_EDGE('',*,*,#1968,.T.);
#2499=ORIENTED_EDGE('',*,*,#1970,.F.);
#2500=ORIENTED_EDGE('',*,*,#1971,.T.);
#2501=ORIENTED_EDGE('',*,*,#1967,.F.);
#2502=ORIENTED_EDGE('',*,*,#1972,.T.);
#2503=ORIENTED_EDGE('',*,*,#1970,.T.);
#2504=ORIENTED_EDGE('',*,*,#1972,.F.);
#2505=ORIENTED_EDGE('',*,*,#1971,.F.);
#2506=ORIENTED_EDGE('',*,*,#1973,.T.);
#2507=ORIENTED_EDGE('',*,*,#1974,.T.);
#2508=ORIENTED_EDGE('',*,*,#1973,.F.);
#2509=ORIENTED_EDGE('',*,*,#1974,.F.);
#2510=ORIENTED_EDGE('',*,*,#1963,.T.);
#2511=ORIENTED_EDGE('',*,*,#1975,.F.);
#2512=ORIENTED_EDGE('',*,*,#1976,.T.);
#2513=ORIENTED_EDGE('',*,*,#1977,.F.);
#2514=ORIENTED_EDGE('',*,*,#1978,.F.);
#2515=ORIENTED_EDGE('',*,*,#1979,.F.);
#2516=ORIENTED_EDGE('',*,*,#1980,.F.);
#2517=ORIENTED_EDGE('',*,*,#1981,.F.);
#2518=ORIENTED_EDGE('',*,*,#1976,.F.);
#2519=ORIENTED_EDGE('',*,*,#1982,.F.);
#2520=ORIENTED_EDGE('',*,*,#1983,.T.);
#2521=ORIENTED_EDGE('',*,*,#1984,.F.);
#2522=ORIENTED_EDGE('',*,*,#1985,.F.);
#2523=ORIENTED_EDGE('',*,*,#1986,.F.);
#2524=ORIENTED_EDGE('',*,*,#1987,.F.);
#2525=ORIENTED_EDGE('',*,*,#1988,.F.);
#2526=ORIENTED_EDGE('',*,*,#1983,.F.);
#2527=ORIENTED_EDGE('',*,*,#1989,.F.);
#2528=ORIENTED_EDGE('',*,*,#1990,.T.);
#2529=ORIENTED_EDGE('',*,*,#1991,.F.);
#2530=ORIENTED_EDGE('',*,*,#1992,.F.);
#2531=ORIENTED_EDGE('',*,*,#1993,.F.);
#2532=ORIENTED_EDGE('',*,*,#1994,.F.);
#2533=ORIENTED_EDGE('',*,*,#1995,.F.);
#2534=ORIENTED_EDGE('',*,*,#1990,.F.);
#2535=ORIENTED_EDGE('',*,*,#1996,.F.);
#2536=ORIENTED_EDGE('',*,*,#1997,.T.);
#2537=ORIENTED_EDGE('',*,*,#1998,.F.);
#2538=ORIENTED_EDGE('',*,*,#1999,.F.);
#2539=ORIENTED_EDGE('',*,*,#2000,.F.);
#2540=ORIENTED_EDGE('',*,*,#2001,.F.);
#2541=ORIENTED_EDGE('',*,*,#2002,.F.);
#2542=ORIENTED_EDGE('',*,*,#1997,.F.);
#2543=ORIENTED_EDGE('',*,*,#2003,.F.);
#2544=ORIENTED_EDGE('',*,*,#2004,.T.);
#2545=ORIENTED_EDGE('',*,*,#2005,.F.);
#2546=ORIENTED_EDGE('',*,*,#2006,.F.);
#2547=ORIENTED_EDGE('',*,*,#2007,.F.);
#2548=ORIENTED_EDGE('',*,*,#2008,.F.);
#2549=ORIENTED_EDGE('',*,*,#2009,.F.);
#2550=ORIENTED_EDGE('',*,*,#2004,.F.);
#2551=ORIENTED_EDGE('',*,*,#2010,.F.);
#2552=ORIENTED_EDGE('',*,*,#2011,.T.);
#2553=ORIENTED_EDGE('',*,*,#2012,.F.);
#2554=ORIENTED_EDGE('',*,*,#2013,.F.);
#2555=ORIENTED_EDGE('',*,*,#2014,.F.);
#2556=ORIENTED_EDGE('',*,*,#2015,.F.);
#2557=ORIENTED_EDGE('',*,*,#2016,.F.);
#2558=ORIENTED_EDGE('',*,*,#2011,.F.);
#2559=ORIENTED_EDGE('',*,*,#2017,.F.);
#2560=ORIENTED_EDGE('',*,*,#2018,.T.);
#2561=ORIENTED_EDGE('',*,*,#2019,.F.);
#2562=ORIENTED_EDGE('',*,*,#2020,.F.);
#2563=ORIENTED_EDGE('',*,*,#2021,.F.);
#2564=ORIENTED_EDGE('',*,*,#2022,.F.);
#2565=ORIENTED_EDGE('',*,*,#2023,.F.);
#2566=ORIENTED_EDGE('',*,*,#2018,.F.);
#2567=ORIENTED_EDGE('',*,*,#2024,.F.);
#2568=ORIENTED_EDGE('',*,*,#2025,.T.);
#2569=ORIENTED_EDGE('',*,*,#2026,.F.);
#2570=ORIENTED_EDGE('',*,*,#2027,.F.);
#2571=ORIENTED_EDGE('',*,*,#2028,.F.);
#2572=ORIENTED_EDGE('',*,*,#2029,.F.);
#2573=ORIENTED_EDGE('',*,*,#2030,.F.);
#2574=ORIENTED_EDGE('',*,*,#2025,.F.);
#2575=ORIENTED_EDGE('',*,*,#2031,.F.);
#2576=ORIENTED_EDGE('',*,*,#2032,.T.);
#2577=ORIENTED_EDGE('',*,*,#2033,.F.);
#2578=ORIENTED_EDGE('',*,*,#2034,.F.);
#2579=ORIENTED_EDGE('',*,*,#2035,.F.);
#2580=ORIENTED_EDGE('',*,*,#2036,.F.);
#2581=ORIENTED_EDGE('',*,*,#2037,.F.);
#2582=ORIENTED_EDGE('',*,*,#2032,.F.);
#2583=ORIENTED_EDGE('',*,*,#2038,.F.);
#2584=ORIENTED_EDGE('',*,*,#2039,.T.);
#2585=ORIENTED_EDGE('',*,*,#2040,.F.);
#2586=ORIENTED_EDGE('',*,*,#2041,.F.);
#2587=ORIENTED_EDGE('',*,*,#2042,.F.);
#2588=ORIENTED_EDGE('',*,*,#2043,.F.);
#2589=ORIENTED_EDGE('',*,*,#2044,.F.);
#2590=ORIENTED_EDGE('',*,*,#2039,.F.);
#2591=ORIENTED_EDGE('',*,*,#1978,.T.);
#2592=ORIENTED_EDGE('',*,*,#2045,.T.);
#2593=ORIENTED_EDGE('',*,*,#2034,.T.);
#2594=ORIENTED_EDGE('',*,*,#2046,.T.);
#2595=ORIENTED_EDGE('',*,*,#1986,.T.);
#2596=ORIENTED_EDGE('',*,*,#2047,.T.);
#2597=ORIENTED_EDGE('',*,*,#2028,.T.);
#2598=ORIENTED_EDGE('',*,*,#2048,.T.);
#2599=ORIENTED_EDGE('',*,*,#2021,.T.);
#2600=ORIENTED_EDGE('',*,*,#2049,.T.);
#2601=ORIENTED_EDGE('',*,*,#2001,.T.);
#2602=ORIENTED_EDGE('',*,*,#2050,.T.);
#2603=ORIENTED_EDGE('',*,*,#2015,.T.);
#2604=ORIENTED_EDGE('',*,*,#2051,.T.);
#2605=ORIENTED_EDGE('',*,*,#2008,.T.);
#2606=ORIENTED_EDGE('',*,*,#2052,.T.);
#2607=ORIENTED_EDGE('',*,*,#1991,.T.);
#2608=ORIENTED_EDGE('',*,*,#1995,.T.);
#2609=ORIENTED_EDGE('',*,*,#2053,.T.);
#2610=ORIENTED_EDGE('',*,*,#2041,.T.);
#2611=ORIENTED_EDGE('',*,*,#2054,.T.);
#2612=ORIENTED_EDGE('',*,*,#2055,.T.);
#2613=ORIENTED_EDGE('',*,*,#2022,.T.);
#2614=ORIENTED_EDGE('',*,*,#2048,.F.);
#2615=ORIENTED_EDGE('',*,*,#2027,.T.);
#2616=ORIENTED_EDGE('',*,*,#2056,.F.);
#2617=ORIENTED_EDGE('',*,*,#2005,.T.);
#2618=ORIENTED_EDGE('',*,*,#2009,.T.);
#2619=ORIENTED_EDGE('',*,*,#2051,.F.);
#2620=ORIENTED_EDGE('',*,*,#2014,.T.);
#2621=ORIENTED_EDGE('',*,*,#2057,.F.);
#2622=ORIENTED_EDGE('',*,*,#1998,.T.);
#2623=ORIENTED_EDGE('',*,*,#2002,.T.);
#2624=ORIENTED_EDGE('',*,*,#2049,.F.);
#2625=ORIENTED_EDGE('',*,*,#2020,.T.);
#2626=ORIENTED_EDGE('',*,*,#2058,.F.);
#2627=ORIENTED_EDGE('',*,*,#2000,.T.);
#2628=ORIENTED_EDGE('',*,*,#2059,.F.);
#2629=ORIENTED_EDGE('',*,*,#2012,.T.);
#2630=ORIENTED_EDGE('',*,*,#2016,.T.);
#2631=ORIENTED_EDGE('',*,*,#2050,.F.);
#2632=ORIENTED_EDGE('',*,*,#1992,.T.);
#2633=ORIENTED_EDGE('',*,*,#2052,.F.);
#2634=ORIENTED_EDGE('',*,*,#2007,.T.);
#2635=ORIENTED_EDGE('',*,*,#2060,.F.);
#2636=ORIENTED_EDGE('',*,*,#1994,.T.);
#2637=ORIENTED_EDGE('',*,*,#2061,.F.);
#2638=ORIENTED_EDGE('',*,*,#2042,.T.);
#2639=ORIENTED_EDGE('',*,*,#2053,.F.);
#2640=ORIENTED_EDGE('',*,*,#1987,.T.);
#2641=ORIENTED_EDGE('',*,*,#2046,.F.);
#2642=ORIENTED_EDGE('',*,*,#2033,.T.);
#2643=ORIENTED_EDGE('',*,*,#2037,.T.);
#2644=ORIENTED_EDGE('',*,*,#2062,.F.);
#2645=ORIENTED_EDGE('',*,*,#1985,.T.);
#2646=ORIENTED_EDGE('',*,*,#2063,.F.);
#2647=ORIENTED_EDGE('',*,*,#2029,.T.);
#2648=ORIENTED_EDGE('',*,*,#2047,.F.);
#2649=ORIENTED_EDGE('',*,*,#1979,.T.);
#2650=ORIENTED_EDGE('',*,*,#2054,.F.);
#2651=ORIENTED_EDGE('',*,*,#2040,.T.);
#2652=ORIENTED_EDGE('',*,*,#2044,.T.);
#2653=ORIENTED_EDGE('',*,*,#2064,.F.);
#2654=ORIENTED_EDGE('',*,*,#1977,.T.);
#2655=ORIENTED_EDGE('',*,*,#1981,.T.);
#2656=ORIENTED_EDGE('',*,*,#2065,.F.);
#2657=ORIENTED_EDGE('',*,*,#2035,.T.);
#2658=ORIENTED_EDGE('',*,*,#2045,.F.);
#2659=ORIENTED_EDGE('',*,*,#2066,.F.);
#2660=ORIENTED_EDGE('',*,*,#1980,.T.);
#2661=ORIENTED_EDGE('',*,*,#2064,.T.);
#2662=ORIENTED_EDGE('',*,*,#2043,.T.);
#2663=ORIENTED_EDGE('',*,*,#2061,.T.);
#2664=ORIENTED_EDGE('',*,*,#1993,.T.);
#2665=ORIENTED_EDGE('',*,*,#2060,.T.);
#2666=ORIENTED_EDGE('',*,*,#2006,.T.);
#2667=ORIENTED_EDGE('',*,*,#2057,.T.);
#2668=ORIENTED_EDGE('',*,*,#2013,.T.);
#2669=ORIENTED_EDGE('',*,*,#2059,.T.);
#2670=ORIENTED_EDGE('',*,*,#1999,.T.);
#2671=ORIENTED_EDGE('',*,*,#2058,.T.);
#2672=ORIENTED_EDGE('',*,*,#2019,.T.);
#2673=ORIENTED_EDGE('',*,*,#2023,.T.);
#2674=ORIENTED_EDGE('',*,*,#2056,.T.);
#2675=ORIENTED_EDGE('',*,*,#2026,.T.);
#2676=ORIENTED_EDGE('',*,*,#2030,.T.);
#2677=ORIENTED_EDGE('',*,*,#2063,.T.);
#2678=ORIENTED_EDGE('',*,*,#1984,.T.);
#2679=ORIENTED_EDGE('',*,*,#1988,.T.);
#2680=ORIENTED_EDGE('',*,*,#2062,.T.);
#2681=ORIENTED_EDGE('',*,*,#2036,.T.);
#2682=ORIENTED_EDGE('',*,*,#2065,.T.);
#2683=ORIENTED_EDGE('',*,*,#2067,.F.);
#2684=ORIENTED_EDGE('',*,*,#2068,.T.);
#2685=ORIENTED_EDGE('',*,*,#2066,.T.);
#2686=ORIENTED_EDGE('',*,*,#2068,.F.);
#2687=ORIENTED_EDGE('',*,*,#2067,.T.);
#2688=ORIENTED_EDGE('',*,*,#2069,.F.);
#2689=ORIENTED_EDGE('',*,*,#2038,.T.);
#2690=ORIENTED_EDGE('',*,*,#2031,.T.);
#2691=ORIENTED_EDGE('',*,*,#2024,.T.);
#2692=ORIENTED_EDGE('',*,*,#2017,.T.);
#2693=ORIENTED_EDGE('',*,*,#2010,.T.);
#2694=ORIENTED_EDGE('',*,*,#2003,.T.);
#2695=ORIENTED_EDGE('',*,*,#1996,.T.);
#2696=ORIENTED_EDGE('',*,*,#1989,.T.);
#2697=ORIENTED_EDGE('',*,*,#1982,.T.);
#2698=ORIENTED_EDGE('',*,*,#1975,.T.);
#2699=ORIENTED_EDGE('',*,*,#2069,.T.);
#2700=ORIENTED_EDGE('',*,*,#2070,.T.);
#2701=ORIENTED_EDGE('',*,*,#2055,.F.);
#2702=ORIENTED_EDGE('',*,*,#2070,.F.);
#2703=ORIENTED_EDGE('',*,*,#2071,.F.);
#2704=ORIENTED_EDGE('',*,*,#2072,.F.);
#2705=ORIENTED_EDGE('',*,*,#2073,.F.);
#2706=ORIENTED_EDGE('',*,*,#2074,.T.);
#2707=ORIENTED_EDGE('',*,*,#2075,.F.);
#2708=ORIENTED_EDGE('',*,*,#2074,.F.);
#2709=ORIENTED_EDGE('',*,*,#2076,.F.);
#2710=ORIENTED_EDGE('',*,*,#2077,.F.);
#2711=ORIENTED_EDGE('',*,*,#2078,.F.);
#2712=ORIENTED_EDGE('',*,*,#2079,.F.);
#2713=ORIENTED_EDGE('',*,*,#2080,.F.);
#2714=ORIENTED_EDGE('',*,*,#2081,.F.);
#2715=ORIENTED_EDGE('',*,*,#2082,.T.);
#2716=ORIENTED_EDGE('',*,*,#2083,.F.);
#2717=ORIENTED_EDGE('',*,*,#2082,.F.);
#2718=ORIENTED_EDGE('',*,*,#2084,.F.);
#2719=ORIENTED_EDGE('',*,*,#2085,.F.);
#2720=ORIENTED_EDGE('',*,*,#2086,.F.);
#2721=ORIENTED_EDGE('',*,*,#2087,.T.);
#2722=ORIENTED_EDGE('',*,*,#2088,.F.);
#2723=ORIENTED_EDGE('',*,*,#2087,.F.);
#2724=ORIENTED_EDGE('',*,*,#2089,.F.);
#2725=ORIENTED_EDGE('',*,*,#2090,.F.);
#2726=ORIENTED_EDGE('',*,*,#2091,.F.);
#2727=ORIENTED_EDGE('',*,*,#2092,.F.);
#2728=ORIENTED_EDGE('',*,*,#2093,.F.);
#2729=ORIENTED_EDGE('',*,*,#2094,.F.);
#2730=ORIENTED_EDGE('',*,*,#2095,.F.);
#2731=ORIENTED_EDGE('',*,*,#2096,.F.);
#2732=ORIENTED_EDGE('',*,*,#2097,.T.);
#2733=ORIENTED_EDGE('',*,*,#2098,.F.);
#2734=ORIENTED_EDGE('',*,*,#2097,.F.);
#2735=ORIENTED_EDGE('',*,*,#2099,.F.);
#2736=ORIENTED_EDGE('',*,*,#2100,.F.);
#2737=ORIENTED_EDGE('',*,*,#2101,.F.);
#2738=ORIENTED_EDGE('',*,*,#2102,.F.);
#2739=ORIENTED_EDGE('',*,*,#2103,.F.);
#2740=ORIENTED_EDGE('',*,*,#2104,.T.);
#2741=ORIENTED_EDGE('',*,*,#2105,.F.);
#2742=ORIENTED_EDGE('',*,*,#2104,.F.);
#2743=ORIENTED_EDGE('',*,*,#2106,.F.);
#2744=ORIENTED_EDGE('',*,*,#2107,.F.);
#2745=ORIENTED_EDGE('',*,*,#2108,.F.);
#2746=ORIENTED_EDGE('',*,*,#2109,.F.);
#2747=ORIENTED_EDGE('',*,*,#2110,.F.);
#2748=ORIENTED_EDGE('',*,*,#2111,.T.);
#2749=ORIENTED_EDGE('',*,*,#2112,.F.);
#2750=ORIENTED_EDGE('',*,*,#2111,.F.);
#2751=ORIENTED_EDGE('',*,*,#2113,.F.);
#2752=ORIENTED_EDGE('',*,*,#2114,.F.);
#2753=ORIENTED_EDGE('',*,*,#2115,.F.);
#2754=ORIENTED_EDGE('',*,*,#2116,.F.);
#2755=ORIENTED_EDGE('',*,*,#2117,.T.);
#2756=ORIENTED_EDGE('',*,*,#2118,.F.);
#2757=ORIENTED_EDGE('',*,*,#2117,.F.);
#2758=ORIENTED_EDGE('',*,*,#2119,.F.);
#2759=ORIENTED_EDGE('',*,*,#2120,.F.);
#2760=ORIENTED_EDGE('',*,*,#2121,.F.);
#2761=ORIENTED_EDGE('',*,*,#2122,.F.);
#2762=ORIENTED_EDGE('',*,*,#2123,.F.);
#2763=ORIENTED_EDGE('',*,*,#2124,.T.);
#2764=ORIENTED_EDGE('',*,*,#2125,.F.);
#2765=ORIENTED_EDGE('',*,*,#2124,.F.);
#2766=ORIENTED_EDGE('',*,*,#2126,.F.);
#2767=ORIENTED_EDGE('',*,*,#2127,.F.);
#2768=ORIENTED_EDGE('',*,*,#2128,.F.);
#2769=ORIENTED_EDGE('',*,*,#2129,.F.);
#2770=ORIENTED_EDGE('',*,*,#2130,.T.);
#2771=ORIENTED_EDGE('',*,*,#2131,.F.);
#2772=ORIENTED_EDGE('',*,*,#2130,.F.);
#2773=ORIENTED_EDGE('',*,*,#2132,.F.);
#2774=ORIENTED_EDGE('',*,*,#2133,.F.);
#2775=ORIENTED_EDGE('',*,*,#2134,.F.);
#2776=ORIENTED_EDGE('',*,*,#2135,.F.);
#2777=ORIENTED_EDGE('',*,*,#2136,.F.);
#2778=ORIENTED_EDGE('',*,*,#2137,.T.);
#2779=ORIENTED_EDGE('',*,*,#2138,.F.);
#2780=ORIENTED_EDGE('',*,*,#2137,.F.);
#2781=ORIENTED_EDGE('',*,*,#2139,.F.);
#2782=ORIENTED_EDGE('',*,*,#2140,.F.);
#2783=ORIENTED_EDGE('',*,*,#2072,.T.);
#2784=ORIENTED_EDGE('',*,*,#2141,.T.);
#2785=ORIENTED_EDGE('',*,*,#2135,.T.);
#2786=ORIENTED_EDGE('',*,*,#2142,.T.);
#2787=ORIENTED_EDGE('',*,*,#2089,.T.);
#2788=ORIENTED_EDGE('',*,*,#2086,.T.);
#2789=ORIENTED_EDGE('',*,*,#2143,.T.);
#2790=ORIENTED_EDGE('',*,*,#2100,.T.);
#2791=ORIENTED_EDGE('',*,*,#2144,.T.);
#2792=ORIENTED_EDGE('',*,*,#2107,.T.);
#2793=ORIENTED_EDGE('',*,*,#2145,.T.);
#2794=ORIENTED_EDGE('',*,*,#2093,.T.);
#2795=ORIENTED_EDGE('',*,*,#2146,.T.);
#2796=ORIENTED_EDGE('',*,*,#2114,.T.);
#2797=ORIENTED_EDGE('',*,*,#2147,.T.);
#2798=ORIENTED_EDGE('',*,*,#2121,.T.);
#2799=ORIENTED_EDGE('',*,*,#2148,.T.);
#2800=ORIENTED_EDGE('',*,*,#2079,.T.);
#2801=ORIENTED_EDGE('',*,*,#2149,.T.);
#2802=ORIENTED_EDGE('',*,*,#2128,.T.);
#2803=ORIENTED_EDGE('',*,*,#2150,.T.);
#2804=ORIENTED_EDGE('',*,*,#2151,.F.);
#2805=ORIENTED_EDGE('',*,*,#2113,.T.);
#2806=ORIENTED_EDGE('',*,*,#2152,.F.);
#2807=ORIENTED_EDGE('',*,*,#2122,.T.);
#2808=ORIENTED_EDGE('',*,*,#2147,.F.);
#2809=ORIENTED_EDGE('',*,*,#2099,.T.);
#2810=ORIENTED_EDGE('',*,*,#2103,.T.);
#2811=ORIENTED_EDGE('',*,*,#2153,.F.);
#2812=ORIENTED_EDGE('',*,*,#2108,.T.);
#2813=ORIENTED_EDGE('',*,*,#2144,.F.);
#2814=ORIENTED_EDGE('',*,*,#2092,.T.);
#2815=ORIENTED_EDGE('',*,*,#2096,.T.);
#2816=ORIENTED_EDGE('',*,*,#2154,.F.);
#2817=ORIENTED_EDGE('',*,*,#2115,.T.);
#2818=ORIENTED_EDGE('',*,*,#2146,.F.);
#2819=ORIENTED_EDGE('',*,*,#2094,.T.);
#2820=ORIENTED_EDGE('',*,*,#2145,.F.);
#2821=ORIENTED_EDGE('',*,*,#2106,.T.);
#2822=ORIENTED_EDGE('',*,*,#2110,.T.);
#2823=ORIENTED_EDGE('',*,*,#2155,.F.);
#2824=ORIENTED_EDGE('',*,*,#2085,.T.);
#2825=ORIENTED_EDGE('',*,*,#2156,.F.);
#2826=ORIENTED_EDGE('',*,*,#2101,.T.);
#2827=ORIENTED_EDGE('',*,*,#2143,.F.);
#2828=ORIENTED_EDGE('',*,*,#2090,.T.);
#2829=ORIENTED_EDGE('',*,*,#2142,.F.);
#2830=ORIENTED_EDGE('',*,*,#2134,.T.);
#2831=ORIENTED_EDGE('',*,*,#2157,.F.);
#2832=ORIENTED_EDGE('',*,*,#2078,.T.);
#2833=ORIENTED_EDGE('',*,*,#2158,.F.);
#2834=ORIENTED_EDGE('',*,*,#2132,.T.);
#2835=ORIENTED_EDGE('',*,*,#2129,.T.);
#2836=ORIENTED_EDGE('',*,*,#2149,.F.);
#2837=ORIENTED_EDGE('',*,*,#2080,.T.);
#2838=ORIENTED_EDGE('',*,*,#2148,.F.);
#2839=ORIENTED_EDGE('',*,*,#2120,.T.);
#2840=ORIENTED_EDGE('',*,*,#2159,.F.);
#2841=ORIENTED_EDGE('',*,*,#2071,.T.);
#2842=ORIENTED_EDGE('',*,*,#2160,.F.);
#2843=ORIENTED_EDGE('',*,*,#2139,.T.);
#2844=ORIENTED_EDGE('',*,*,#2136,.T.);
#2845=ORIENTED_EDGE('',*,*,#2141,.F.);
#2846=ORIENTED_EDGE('',*,*,#2076,.T.);
#2847=ORIENTED_EDGE('',*,*,#2073,.T.);
#2848=ORIENTED_EDGE('',*,*,#2150,.F.);
#2849=ORIENTED_EDGE('',*,*,#2127,.T.);
#2850=ORIENTED_EDGE('',*,*,#2161,.F.);
#2851=ORIENTED_EDGE('',*,*,#2162,.F.);
#2852=ORIENTED_EDGE('',*,*,#2163,.T.);
#2853=ORIENTED_EDGE('',*,*,#2138,.T.);
#2854=ORIENTED_EDGE('',*,*,#2131,.T.);
#2855=ORIENTED_EDGE('',*,*,#2125,.T.);
#2856=ORIENTED_EDGE('',*,*,#2118,.T.);
#2857=ORIENTED_EDGE('',*,*,#2112,.T.);
#2858=ORIENTED_EDGE('',*,*,#2105,.T.);
#2859=ORIENTED_EDGE('',*,*,#2098,.T.);
#2860=ORIENTED_EDGE('',*,*,#2088,.T.);
#2861=ORIENTED_EDGE('',*,*,#2083,.T.);
#2862=ORIENTED_EDGE('',*,*,#2075,.T.);
#2863=ORIENTED_EDGE('',*,*,#2164,.F.);
#2864=ORIENTED_EDGE('',*,*,#2165,.T.);
#2865=ORIENTED_EDGE('',*,*,#2162,.T.);
#2866=ORIENTED_EDGE('',*,*,#2165,.F.);
#2867=ORIENTED_EDGE('',*,*,#2164,.T.);
#2868=ORIENTED_EDGE('',*,*,#2077,.T.);
#2869=ORIENTED_EDGE('',*,*,#2161,.T.);
#2870=ORIENTED_EDGE('',*,*,#2133,.T.);
#2871=ORIENTED_EDGE('',*,*,#2158,.T.);
#2872=ORIENTED_EDGE('',*,*,#2084,.T.);
#2873=ORIENTED_EDGE('',*,*,#2081,.T.);
#2874=ORIENTED_EDGE('',*,*,#2159,.T.);
#2875=ORIENTED_EDGE('',*,*,#2126,.T.);
#2876=ORIENTED_EDGE('',*,*,#2123,.T.);
#2877=ORIENTED_EDGE('',*,*,#2152,.T.);
#2878=ORIENTED_EDGE('',*,*,#2119,.T.);
#2879=ORIENTED_EDGE('',*,*,#2116,.T.);
#2880=ORIENTED_EDGE('',*,*,#2154,.T.);
#2881=ORIENTED_EDGE('',*,*,#2095,.T.);
#2882=ORIENTED_EDGE('',*,*,#2155,.T.);
#2883=ORIENTED_EDGE('',*,*,#2109,.T.);
#2884=ORIENTED_EDGE('',*,*,#2153,.T.);
#2885=ORIENTED_EDGE('',*,*,#2102,.T.);
#2886=ORIENTED_EDGE('',*,*,#2156,.T.);
#2887=ORIENTED_EDGE('',*,*,#2091,.T.);
#2888=ORIENTED_EDGE('',*,*,#2157,.T.);
#2889=ORIENTED_EDGE('',*,*,#2140,.T.);
#2890=ORIENTED_EDGE('',*,*,#2160,.T.);
#2891=ORIENTED_EDGE('',*,*,#2151,.T.);
#2892=ORIENTED_EDGE('',*,*,#2166,.T.);
#2893=ORIENTED_EDGE('',*,*,#2163,.F.);
#2894=ORIENTED_EDGE('',*,*,#2166,.F.);
#2895=ORIENTED_EDGE('',*,*,#2167,.T.);
#2896=ORIENTED_EDGE('',*,*,#2167,.F.);
#2897=ORIENTED_EDGE('',*,*,#2168,.T.);
#2898=ORIENTED_EDGE('',*,*,#2168,.F.);
#2899=ORIENTED_EDGE('',*,*,#2169,.T.);
#2900=ORIENTED_EDGE('',*,*,#2169,.F.);
#2901=ORIENTED_EDGE('',*,*,#2170,.T.);
#2902=ORIENTED_EDGE('',*,*,#2170,.F.);
#2903=ORIENTED_EDGE('',*,*,#2171,.T.);
#2904=ORIENTED_EDGE('',*,*,#2171,.F.);
#2905=ORIENTED_EDGE('',*,*,#2172,.T.);
#2906=ORIENTED_EDGE('',*,*,#2172,.F.);
#2907=ORIENTED_EDGE('',*,*,#2173,.T.);
#2908=ORIENTED_EDGE('',*,*,#2173,.F.);
#2909=ORIENTED_EDGE('',*,*,#2174,.T.);
#2910=ORIENTED_EDGE('',*,*,#2174,.F.);
#2911=ORIENTED_EDGE('',*,*,#2175,.T.);
#2912=ORIENTED_EDGE('',*,*,#2175,.F.);
#2913=ORIENTED_EDGE('',*,*,#2176,.T.);
#2914=ORIENTED_EDGE('',*,*,#2176,.F.);
#2915=ORIENTED_EDGE('',*,*,#2177,.F.);
#2916=ORIENTED_EDGE('',*,*,#2178,.T.);
#2917=ORIENTED_EDGE('',*,*,#2179,.T.);
#2918=ORIENTED_EDGE('',*,*,#2178,.F.);
#2919=ORIENTED_EDGE('',*,*,#2180,.F.);
#2920=ORIENTED_EDGE('',*,*,#2181,.T.);
#2921=ORIENTED_EDGE('',*,*,#2182,.T.);
#2922=ORIENTED_EDGE('',*,*,#2181,.F.);
#2923=ORIENTED_EDGE('',*,*,#2180,.T.);
#2924=ORIENTED_EDGE('',*,*,#2177,.T.);
#2925=ORIENTED_EDGE('',*,*,#2182,.F.);
#2926=ORIENTED_EDGE('',*,*,#2179,.F.);
#2927=ORIENTED_EDGE('',*,*,#2183,.F.);
#2928=ORIENTED_EDGE('',*,*,#2184,.F.);
#2929=ORIENTED_EDGE('',*,*,#2185,.T.);
#2930=ORIENTED_EDGE('',*,*,#2186,.F.);
#2931=ORIENTED_EDGE('',*,*,#2185,.F.);
#2932=ORIENTED_EDGE('',*,*,#2187,.F.);
#2933=ORIENTED_EDGE('',*,*,#2188,.F.);
#2934=ORIENTED_EDGE('',*,*,#2189,.F.);
#2935=ORIENTED_EDGE('',*,*,#2190,.F.);
#2936=ORIENTED_EDGE('',*,*,#2191,.F.);
#2937=ORIENTED_EDGE('',*,*,#2192,.T.);
#2938=ORIENTED_EDGE('',*,*,#2193,.F.);
#2939=ORIENTED_EDGE('',*,*,#2194,.F.);
#2940=ORIENTED_EDGE('',*,*,#2195,.F.);
#2941=ORIENTED_EDGE('',*,*,#2196,.F.);
#2942=ORIENTED_EDGE('',*,*,#2197,.F.);
#2943=ORIENTED_EDGE('',*,*,#2198,.F.);
#2944=ORIENTED_EDGE('',*,*,#2192,.F.);
#2945=ORIENTED_EDGE('',*,*,#2188,.T.);
#2946=ORIENTED_EDGE('',*,*,#2199,.T.);
#2947=ORIENTED_EDGE('',*,*,#2197,.T.);
#2948=ORIENTED_EDGE('',*,*,#2200,.F.);
#2949=ORIENTED_EDGE('',*,*,#2187,.T.);
#2950=ORIENTED_EDGE('',*,*,#2201,.T.);
#2951=ORIENTED_EDGE('',*,*,#2198,.T.);
#2952=ORIENTED_EDGE('',*,*,#2199,.F.);
#2953=ORIENTED_EDGE('',*,*,#2184,.T.);
#2954=ORIENTED_EDGE('',*,*,#2202,.T.);
#2955=ORIENTED_EDGE('',*,*,#2193,.T.);
#2956=ORIENTED_EDGE('',*,*,#2201,.F.);
#2957=ORIENTED_EDGE('',*,*,#2203,.F.);
#2958=ORIENTED_EDGE('',*,*,#2204,.T.);
#2959=ORIENTED_EDGE('',*,*,#2205,.T.);
#2960=ORIENTED_EDGE('',*,*,#2204,.F.);
#2961=ORIENTED_EDGE('',*,*,#2183,.T.);
#2962=ORIENTED_EDGE('',*,*,#2206,.T.);
#2963=ORIENTED_EDGE('',*,*,#2194,.T.);
#2964=ORIENTED_EDGE('',*,*,#2202,.F.);
#2965=ORIENTED_EDGE('',*,*,#2189,.T.);
#2966=ORIENTED_EDGE('',*,*,#2200,.T.);
#2967=ORIENTED_EDGE('',*,*,#2196,.T.);
#2968=ORIENTED_EDGE('',*,*,#2207,.F.);
#2969=ORIENTED_EDGE('',*,*,#2190,.T.);
#2970=ORIENTED_EDGE('',*,*,#2207,.T.);
#2971=ORIENTED_EDGE('',*,*,#2195,.T.);
#2972=ORIENTED_EDGE('',*,*,#2206,.F.);
#2973=ORIENTED_EDGE('',*,*,#2191,.T.);
#2974=ORIENTED_EDGE('',*,*,#2203,.T.);
#2975=ORIENTED_EDGE('',*,*,#2186,.T.);
#2976=ORIENTED_EDGE('',*,*,#2205,.F.);
#2977=ORIENTED_EDGE('',*,*,#2208,.F.);
#2978=ORIENTED_EDGE('',*,*,#2209,.T.);
#2979=ORIENTED_EDGE('',*,*,#2210,.F.);
#2980=ORIENTED_EDGE('',*,*,#2209,.F.);
#2981=ORIENTED_EDGE('',*,*,#2211,.F.);
#2982=ORIENTED_EDGE('',*,*,#2212,.F.);
#2983=ORIENTED_EDGE('',*,*,#2213,.F.);
#2984=ORIENTED_EDGE('',*,*,#2214,.F.);
#2985=ORIENTED_EDGE('',*,*,#2215,.F.);
#2986=ORIENTED_EDGE('',*,*,#2216,.F.);
#2987=ORIENTED_EDGE('',*,*,#2217,.F.);
#2988=ORIENTED_EDGE('',*,*,#2218,.F.);
#2989=ORIENTED_EDGE('',*,*,#2216,.T.);
#2990=ORIENTED_EDGE('',*,*,#2219,.T.);
#2991=ORIENTED_EDGE('',*,*,#2220,.T.);
#2992=ORIENTED_EDGE('',*,*,#2221,.T.);
#2993=ORIENTED_EDGE('',*,*,#2222,.T.);
#2994=ORIENTED_EDGE('',*,*,#2223,.F.);
#2995=ORIENTED_EDGE('',*,*,#2224,.F.);
#2996=ORIENTED_EDGE('',*,*,#2225,.T.);
#2997=ORIENTED_EDGE('',*,*,#2226,.T.);
#2998=ORIENTED_EDGE('',*,*,#2227,.T.);
#2999=ORIENTED_EDGE('',*,*,#2215,.T.);
#3000=ORIENTED_EDGE('',*,*,#2228,.F.);
#3001=ORIENTED_EDGE('',*,*,#2229,.T.);
#3002=ORIENTED_EDGE('',*,*,#2219,.F.);
#3003=ORIENTED_EDGE('',*,*,#2217,.T.);
#3004=ORIENTED_EDGE('',*,*,#2227,.F.);
#3005=ORIENTED_EDGE('',*,*,#2230,.F.);
#3006=ORIENTED_EDGE('',*,*,#2231,.F.);
#3007=ORIENTED_EDGE('',*,*,#2213,.T.);
#3008=ORIENTED_EDGE('',*,*,#2232,.T.);
#3009=ORIENTED_EDGE('',*,*,#2233,.T.);
#3010=ORIENTED_EDGE('',*,*,#2234,.T.);
#3011=ORIENTED_EDGE('',*,*,#2235,.T.);
#3012=ORIENTED_EDGE('',*,*,#2236,.F.);
#3013=ORIENTED_EDGE('',*,*,#2237,.F.);
#3014=ORIENTED_EDGE('',*,*,#2238,.T.);
#3015=ORIENTED_EDGE('',*,*,#2239,.T.);
#3016=ORIENTED_EDGE('',*,*,#2240,.T.);
#3017=ORIENTED_EDGE('',*,*,#2212,.T.);
#3018=ORIENTED_EDGE('',*,*,#2241,.F.);
#3019=ORIENTED_EDGE('',*,*,#2242,.F.);
#3020=ORIENTED_EDGE('',*,*,#2232,.F.);
#3021=ORIENTED_EDGE('',*,*,#2243,.F.);
#3022=ORIENTED_EDGE('',*,*,#2220,.F.);
#3023=ORIENTED_EDGE('',*,*,#2229,.F.);
#3024=ORIENTED_EDGE('',*,*,#2244,.F.);
#3025=ORIENTED_EDGE('',*,*,#2245,.F.);
#3026=ORIENTED_EDGE('',*,*,#2246,.F.);
#3027=ORIENTED_EDGE('',*,*,#2230,.T.);
#3028=ORIENTED_EDGE('',*,*,#2226,.F.);
#3029=ORIENTED_EDGE('',*,*,#2218,.T.);
#3030=ORIENTED_EDGE('',*,*,#2231,.T.);
#3031=ORIENTED_EDGE('',*,*,#2246,.T.);
#3032=ORIENTED_EDGE('',*,*,#2247,.F.);
#3033=ORIENTED_EDGE('',*,*,#2244,.T.);
#3034=ORIENTED_EDGE('',*,*,#2228,.T.);
#3035=ORIENTED_EDGE('',*,*,#2243,.T.);
#3036=ORIENTED_EDGE('',*,*,#2247,.T.);
#3037=ORIENTED_EDGE('',*,*,#2245,.T.);
#3038=ORIENTED_EDGE('',*,*,#2225,.F.);
#3039=ORIENTED_EDGE('',*,*,#2248,.F.);
#3040=ORIENTED_EDGE('',*,*,#2234,.F.);
#3041=ORIENTED_EDGE('',*,*,#2249,.T.);
#3042=ORIENTED_EDGE('',*,*,#2250,.T.);
#3043=ORIENTED_EDGE('',*,*,#2251,.T.);
#3044=ORIENTED_EDGE('',*,*,#2238,.F.);
#3045=ORIENTED_EDGE('',*,*,#2252,.F.);
#3046=ORIENTED_EDGE('',*,*,#2221,.F.);
#3047=ORIENTED_EDGE('',*,*,#2208,.T.);
#3048=ORIENTED_EDGE('',*,*,#2211,.T.);
#3049=ORIENTED_EDGE('',*,*,#2253,.T.);
#3050=ORIENTED_EDGE('',*,*,#2254,.T.);
#3051=ORIENTED_EDGE('',*,*,#2250,.F.);
#3052=ORIENTED_EDGE('',*,*,#2255,.T.);
#3053=ORIENTED_EDGE('',*,*,#2241,.T.);
#3054=ORIENTED_EDGE('',*,*,#2249,.F.);
#3055=ORIENTED_EDGE('',*,*,#2233,.F.);
#3056=ORIENTED_EDGE('',*,*,#2242,.T.);
#3057=ORIENTED_EDGE('',*,*,#2255,.F.);
#3058=ORIENTED_EDGE('',*,*,#2251,.F.);
#3059=ORIENTED_EDGE('',*,*,#2254,.F.);
#3060=ORIENTED_EDGE('',*,*,#2256,.F.);
#3061=ORIENTED_EDGE('',*,*,#2239,.F.);
#3062=ORIENTED_EDGE('',*,*,#2214,.T.);
#3063=ORIENTED_EDGE('',*,*,#2240,.F.);
#3064=ORIENTED_EDGE('',*,*,#2256,.T.);
#3065=ORIENTED_EDGE('',*,*,#2253,.F.);
#3066=ORIENTED_EDGE('',*,*,#2248,.T.);
#3067=ORIENTED_EDGE('',*,*,#2224,.T.);
#3068=ORIENTED_EDGE('',*,*,#2257,.F.);
#3069=ORIENTED_EDGE('',*,*,#2235,.F.);
#3070=ORIENTED_EDGE('',*,*,#2252,.T.);
#3071=ORIENTED_EDGE('',*,*,#2237,.T.);
#3072=ORIENTED_EDGE('',*,*,#2258,.F.);
#3073=ORIENTED_EDGE('',*,*,#2222,.F.);
#3074=ORIENTED_EDGE('',*,*,#2258,.T.);
#3075=ORIENTED_EDGE('',*,*,#2236,.T.);
#3076=ORIENTED_EDGE('',*,*,#2257,.T.);
#3077=ORIENTED_EDGE('',*,*,#2223,.T.);
#3078=ORIENTED_EDGE('',*,*,#2210,.T.);
#3079=ORIENTED_EDGE('',*,*,#2259,.F.);
#3080=ORIENTED_EDGE('',*,*,#2260,.T.);
#3081=ORIENTED_EDGE('',*,*,#2261,.T.);
#3082=ORIENTED_EDGE('',*,*,#2260,.F.);
#3083=ORIENTED_EDGE('',*,*,#2262,.F.);
#3084=ORIENTED_EDGE('',*,*,#2263,.T.);
#3085=ORIENTED_EDGE('',*,*,#2264,.T.);
#3086=ORIENTED_EDGE('',*,*,#2263,.F.);
#3087=ORIENTED_EDGE('',*,*,#2262,.T.);
#3088=ORIENTED_EDGE('',*,*,#2259,.T.);
#3089=ORIENTED_EDGE('',*,*,#2264,.F.);
#3090=ORIENTED_EDGE('',*,*,#2261,.F.);
#3091=ORIENTED_EDGE('',*,*,#2265,.F.);
#3092=ORIENTED_EDGE('',*,*,#2266,.T.);
#3093=ORIENTED_EDGE('',*,*,#2267,.F.);
#3094=ORIENTED_EDGE('',*,*,#2266,.F.);
#3095=ORIENTED_EDGE('',*,*,#2265,.T.);
#3096=ORIENTED_EDGE('',*,*,#2268,.T.);
#3097=ORIENTED_EDGE('',*,*,#2269,.F.);
#3098=ORIENTED_EDGE('',*,*,#2268,.F.);
#3099=ORIENTED_EDGE('',*,*,#2270,.T.);
#3100=ORIENTED_EDGE('',*,*,#2271,.T.);
#3101=ORIENTED_EDGE('',*,*,#2270,.F.);
#3102=ORIENTED_EDGE('',*,*,#2271,.F.);
#3103=ORIENTED_EDGE('',*,*,#2272,.F.);
#3104=ORIENTED_EDGE('',*,*,#2273,.T.);
#3105=ORIENTED_EDGE('',*,*,#2269,.T.);
#3106=ORIENTED_EDGE('',*,*,#2273,.F.);
#3107=ORIENTED_EDGE('',*,*,#2272,.T.);
#3108=ORIENTED_EDGE('',*,*,#2267,.T.);
#3109=ORIENTED_EDGE('',*,*,#2274,.F.);
#3110=ORIENTED_EDGE('',*,*,#2275,.T.);
#3111=ORIENTED_EDGE('',*,*,#2276,.T.);
#3112=ORIENTED_EDGE('',*,*,#2275,.F.);
#3113=ORIENTED_EDGE('',*,*,#2277,.F.);
#3114=ORIENTED_EDGE('',*,*,#2278,.T.);
#3115=ORIENTED_EDGE('',*,*,#2279,.T.);
#3116=ORIENTED_EDGE('',*,*,#2278,.F.);
#3117=ORIENTED_EDGE('',*,*,#2277,.T.);
#3118=ORIENTED_EDGE('',*,*,#2274,.T.);
#3119=ORIENTED_EDGE('',*,*,#2279,.F.);
#3120=ORIENTED_EDGE('',*,*,#2276,.F.);
#3121=ORIENTED_EDGE('',*,*,#2280,.F.);
#3122=ORIENTED_EDGE('',*,*,#2281,.T.);
#3123=ORIENTED_EDGE('',*,*,#2282,.T.);
#3124=ORIENTED_EDGE('',*,*,#2281,.F.);
#3125=ORIENTED_EDGE('',*,*,#2283,.F.);
#3126=ORIENTED_EDGE('',*,*,#2284,.T.);
#3127=ORIENTED_EDGE('',*,*,#2285,.T.);
#3128=ORIENTED_EDGE('',*,*,#2284,.F.);
#3129=ORIENTED_EDGE('',*,*,#2283,.T.);
#3130=ORIENTED_EDGE('',*,*,#2280,.T.);
#3131=ORIENTED_EDGE('',*,*,#2285,.F.);
#3132=ORIENTED_EDGE('',*,*,#2282,.F.);
#3133=ORIENTED_EDGE('',*,*,#2286,.T.);
#3134=ORIENTED_EDGE('',*,*,#2287,.T.);
#3135=ORIENTED_EDGE('',*,*,#2288,.T.);
#3136=ORIENTED_EDGE('',*,*,#2289,.F.);
#3137=ORIENTED_EDGE('',*,*,#2290,.T.);
#3138=ORIENTED_EDGE('',*,*,#2291,.T.);
#3139=ORIENTED_EDGE('',*,*,#2292,.T.);
#3140=ORIENTED_EDGE('',*,*,#2287,.F.);
#3141=ORIENTED_EDGE('',*,*,#2293,.T.);
#3142=ORIENTED_EDGE('',*,*,#2294,.T.);
#3143=ORIENTED_EDGE('',*,*,#2295,.T.);
#3144=ORIENTED_EDGE('',*,*,#2291,.F.);
#3145=ORIENTED_EDGE('',*,*,#2296,.T.);
#3146=ORIENTED_EDGE('',*,*,#2297,.T.);
#3147=ORIENTED_EDGE('',*,*,#2298,.T.);
#3148=ORIENTED_EDGE('',*,*,#2294,.F.);
#3149=ORIENTED_EDGE('',*,*,#2299,.T.);
#3150=ORIENTED_EDGE('',*,*,#2300,.T.);
#3151=ORIENTED_EDGE('',*,*,#2301,.T.);
#3152=ORIENTED_EDGE('',*,*,#2297,.F.);
#3153=ORIENTED_EDGE('',*,*,#2302,.T.);
#3154=ORIENTED_EDGE('',*,*,#2289,.T.);
#3155=ORIENTED_EDGE('',*,*,#2303,.T.);
#3156=ORIENTED_EDGE('',*,*,#2300,.F.);
#3157=ORIENTED_EDGE('',*,*,#2302,.F.);
#3158=ORIENTED_EDGE('',*,*,#2299,.F.);
#3159=ORIENTED_EDGE('',*,*,#2296,.F.);
#3160=ORIENTED_EDGE('',*,*,#2293,.F.);
#3161=ORIENTED_EDGE('',*,*,#2290,.F.);
#3162=ORIENTED_EDGE('',*,*,#2286,.F.);
#3163=ORIENTED_EDGE('',*,*,#2303,.F.);
#3164=ORIENTED_EDGE('',*,*,#2288,.F.);
#3165=ORIENTED_EDGE('',*,*,#2292,.F.);
#3166=ORIENTED_EDGE('',*,*,#2295,.F.);
#3167=ORIENTED_EDGE('',*,*,#2298,.F.);
#3168=ORIENTED_EDGE('',*,*,#2301,.F.);
#3169=ORIENTED_EDGE('',*,*,#2304,.F.);
#3170=ORIENTED_EDGE('',*,*,#2305,.F.);
#3171=ORIENTED_EDGE('',*,*,#2306,.F.);
#3172=ORIENTED_EDGE('',*,*,#2307,.T.);
#3173=ORIENTED_EDGE('',*,*,#2305,.T.);
#3174=ORIENTED_EDGE('',*,*,#2307,.F.);
#3175=ORIENTED_EDGE('',*,*,#2308,.F.);
#3176=ORIENTED_EDGE('',*,*,#2309,.T.);
#3177=ORIENTED_EDGE('',*,*,#2306,.T.);
#3178=ORIENTED_EDGE('',*,*,#2309,.F.);
#3179=ORIENTED_EDGE('',*,*,#2310,.F.);
#3180=ORIENTED_EDGE('',*,*,#2311,.T.);
#3181=ORIENTED_EDGE('',*,*,#2308,.T.);
#3182=ORIENTED_EDGE('',*,*,#2311,.F.);
#3183=ORIENTED_EDGE('',*,*,#2310,.T.);
#3184=ORIENTED_EDGE('',*,*,#2312,.F.);
#3185=ORIENTED_EDGE('',*,*,#2313,.F.);
#3186=ORIENTED_EDGE('',*,*,#2314,.T.);
#3187=ORIENTED_EDGE('',*,*,#2312,.T.);
#3188=ORIENTED_EDGE('',*,*,#2314,.F.);
#3189=ORIENTED_EDGE('',*,*,#2304,.T.);
#3190=ORIENTED_EDGE('',*,*,#2315,.T.);
#3191=ORIENTED_EDGE('',*,*,#2313,.T.);
#3192=ORIENTED_EDGE('',*,*,#2315,.F.);
#3193=ORIENTED_EDGE('',*,*,#2316,.F.);
#3194=ORIENTED_EDGE('',*,*,#2317,.T.);
#3195=ORIENTED_EDGE('',*,*,#2318,.F.);
#3196=ORIENTED_EDGE('',*,*,#2317,.F.);
#3197=ORIENTED_EDGE('',*,*,#2316,.T.);
#3198=ORIENTED_EDGE('',*,*,#2319,.F.);
#3199=ORIENTED_EDGE('',*,*,#2320,.F.);
#3200=ORIENTED_EDGE('',*,*,#2321,.T.);
#3201=ORIENTED_EDGE('',*,*,#2322,.T.);
#3202=ORIENTED_EDGE('',*,*,#2321,.F.);
#3203=ORIENTED_EDGE('',*,*,#2322,.F.);
#3204=ORIENTED_EDGE('',*,*,#2323,.F.);
#3205=ORIENTED_EDGE('',*,*,#2323,.T.);
#3206=ORIENTED_EDGE('',*,*,#2324,.T.);
#3207=ORIENTED_EDGE('',*,*,#2319,.T.);
#3208=ORIENTED_EDGE('',*,*,#2324,.F.);
#3209=ORIENTED_EDGE('',*,*,#2325,.F.);
#3210=ORIENTED_EDGE('',*,*,#2326,.T.);
#3211=ORIENTED_EDGE('',*,*,#2327,.T.);
#3212=ORIENTED_EDGE('',*,*,#2326,.F.);
#3213=ORIENTED_EDGE('',*,*,#2325,.T.);
#3214=ORIENTED_EDGE('',*,*,#2318,.T.);
#3215=ORIENTED_EDGE('',*,*,#2327,.F.);
#3216=ORIENTED_EDGE('',*,*,#2320,.T.);
#3217=ORIENTED_EDGE('',*,*,#2328,.F.);
#3218=ORIENTED_EDGE('',*,*,#2329,.F.);
#3219=ORIENTED_EDGE('',*,*,#2330,.T.);
#3220=ORIENTED_EDGE('',*,*,#2331,.F.);
#3221=ORIENTED_EDGE('',*,*,#2332,.F.);
#3222=ORIENTED_EDGE('',*,*,#2330,.F.);
#3223=ORIENTED_EDGE('',*,*,#2331,.T.);
#3224=ORIENTED_EDGE('',*,*,#2332,.T.);
#3225=ORIENTED_EDGE('',*,*,#2333,.T.);
#3226=ORIENTED_EDGE('',*,*,#2334,.T.);
#3227=ORIENTED_EDGE('',*,*,#2333,.F.);
#3228=ORIENTED_EDGE('',*,*,#2335,.T.);
#3229=ORIENTED_EDGE('',*,*,#2336,.T.);
#3230=ORIENTED_EDGE('',*,*,#2337,.F.);
#3231=ORIENTED_EDGE('',*,*,#2336,.F.);
#3232=ORIENTED_EDGE('',*,*,#2337,.T.);
#3233=ORIENTED_EDGE('',*,*,#2338,.T.);
#3234=ORIENTED_EDGE('',*,*,#2339,.F.);
#3235=ORIENTED_EDGE('',*,*,#2338,.F.);
#3236=ORIENTED_EDGE('',*,*,#2334,.F.);
#3237=ORIENTED_EDGE('',*,*,#2339,.T.);
#3238=ORIENTED_EDGE('',*,*,#2340,.F.);
#3239=ORIENTED_EDGE('',*,*,#2341,.T.);
#3240=ORIENTED_EDGE('',*,*,#2328,.T.);
#3241=ORIENTED_EDGE('',*,*,#2329,.T.);
#3242=ORIENTED_EDGE('',*,*,#2341,.F.);
#3243=ORIENTED_EDGE('',*,*,#2340,.T.);
#3244=ORIENTED_EDGE('',*,*,#2342,.F.);
#3245=ORIENTED_EDGE('',*,*,#2342,.T.);
#3246=ORIENTED_EDGE('',*,*,#2343,.T.);
#3247=ORIENTED_EDGE('',*,*,#2335,.F.);
#3248=ORIENTED_EDGE('',*,*,#2343,.F.);
#3249=ORIENTED_EDGE('',*,*,#2344,.F.);
#3250=ORIENTED_EDGE('',*,*,#2345,.F.);
#3251=ORIENTED_EDGE('',*,*,#2346,.T.);
#3252=ORIENTED_EDGE('',*,*,#2347,.F.);
#3253=ORIENTED_EDGE('',*,*,#2348,.F.);
#3254=ORIENTED_EDGE('',*,*,#2346,.F.);
#3255=ORIENTED_EDGE('',*,*,#2349,.T.);
#3256=ORIENTED_EDGE('',*,*,#2350,.T.);
#3257=ORIENTED_EDGE('',*,*,#2347,.T.);
#3258=ORIENTED_EDGE('',*,*,#2348,.T.);
#3259=ORIENTED_EDGE('',*,*,#2350,.F.);
#3260=ORIENTED_EDGE('',*,*,#2351,.F.);
#3261=ORIENTED_EDGE('',*,*,#2352,.T.);
#3262=ORIENTED_EDGE('',*,*,#2353,.F.);
#3263=ORIENTED_EDGE('',*,*,#2354,.T.);
#3264=ORIENTED_EDGE('',*,*,#2351,.T.);
#3265=ORIENTED_EDGE('',*,*,#2354,.F.);
#3266=ORIENTED_EDGE('',*,*,#2355,.F.);
#3267=ORIENTED_EDGE('',*,*,#2356,.T.);
#3268=ORIENTED_EDGE('',*,*,#2353,.T.);
#3269=ORIENTED_EDGE('',*,*,#2356,.F.);
#3270=ORIENTED_EDGE('',*,*,#2357,.F.);
#3271=ORIENTED_EDGE('',*,*,#2358,.T.);
#3272=ORIENTED_EDGE('',*,*,#2355,.T.);
#3273=ORIENTED_EDGE('',*,*,#2358,.F.);
#3274=ORIENTED_EDGE('',*,*,#2357,.T.);
#3275=ORIENTED_EDGE('',*,*,#2349,.F.);
#3276=ORIENTED_EDGE('',*,*,#2344,.T.);
#3277=ORIENTED_EDGE('',*,*,#2345,.T.);
#3278=ORIENTED_EDGE('',*,*,#2359,.T.);
#3279=ORIENTED_EDGE('',*,*,#2352,.F.);
#3280=ORIENTED_EDGE('',*,*,#2359,.F.);
#3281=ORIENTED_EDGE('',*,*,#2360,.T.);
#3282=ORIENTED_EDGE('',*,*,#2360,.F.);
#3283=ORIENTED_EDGE('',*,*,#2361,.T.);
#3284=ORIENTED_EDGE('',*,*,#2361,.F.);
#3285=ORIENTED_EDGE('',*,*,#2362,.T.);
#3286=ORIENTED_EDGE('',*,*,#2362,.F.);
#3287=ORIENTED_EDGE('',*,*,#2363,.T.);
#3288=ORIENTED_EDGE('',*,*,#2363,.F.);
#3289=ORIENTED_EDGE('',*,*,#2364,.T.);
#3290=ORIENTED_EDGE('',*,*,#2364,.F.);
#3291=ORIENTED_EDGE('',*,*,#2365,.T.);
#3292=ORIENTED_EDGE('',*,*,#2365,.F.);
#3293=ORIENTED_EDGE('',*,*,#2366,.T.);
#3294=ORIENTED_EDGE('',*,*,#2366,.F.);
#3295=ORIENTED_EDGE('',*,*,#2367,.F.);
#3296=ORIENTED_EDGE('',*,*,#2368,.F.);
#3297=ORIENTED_EDGE('',*,*,#2369,.F.);
#3298=ORIENTED_EDGE('',*,*,#2370,.F.);
#3299=ORIENTED_EDGE('',*,*,#2369,.T.);
#3300=ORIENTED_EDGE('',*,*,#2371,.F.);
#3301=ORIENTED_EDGE('',*,*,#2372,.T.);
#3302=ORIENTED_EDGE('',*,*,#2373,.F.);
#3303=ORIENTED_EDGE('',*,*,#2374,.T.);
#3304=ORIENTED_EDGE('',*,*,#2375,.F.);
#3305=ORIENTED_EDGE('',*,*,#2376,.T.);
#3306=ORIENTED_EDGE('',*,*,#2377,.F.);
#3307=ORIENTED_EDGE('',*,*,#2376,.F.);
#3308=ORIENTED_EDGE('',*,*,#2378,.F.);
#3309=ORIENTED_EDGE('',*,*,#2379,.T.);
#3310=ORIENTED_EDGE('',*,*,#2380,.F.);
#3311=ORIENTED_EDGE('',*,*,#2381,.T.);
#3312=ORIENTED_EDGE('',*,*,#2382,.F.);
#3313=ORIENTED_EDGE('',*,*,#2383,.T.);
#3314=ORIENTED_EDGE('',*,*,#2384,.F.);
#3315=ORIENTED_EDGE('',*,*,#2385,.T.);
#3316=ORIENTED_EDGE('',*,*,#2386,.F.);
#3317=ORIENTED_EDGE('',*,*,#2368,.T.);
#3318=ORIENTED_EDGE('',*,*,#2387,.T.);
#3319=ORIENTED_EDGE('',*,*,#2388,.T.);
#3320=ORIENTED_EDGE('',*,*,#2371,.T.);
#3321=ORIENTED_EDGE('',*,*,#2389,.F.);
#3322=ORIENTED_EDGE('',*,*,#2390,.F.);
#3323=ORIENTED_EDGE('',*,*,#2372,.F.);
#3324=ORIENTED_EDGE('',*,*,#2388,.F.);
#3325=ORIENTED_EDGE('',*,*,#2390,.T.);
#3326=ORIENTED_EDGE('',*,*,#2391,.T.);
#3327=ORIENTED_EDGE('',*,*,#2392,.T.);
#3328=ORIENTED_EDGE('',*,*,#2373,.T.);
#3329=ORIENTED_EDGE('',*,*,#2393,.F.);
#3330=ORIENTED_EDGE('',*,*,#2394,.F.);
#3331=ORIENTED_EDGE('',*,*,#2374,.F.);
#3332=ORIENTED_EDGE('',*,*,#2392,.F.);
#3333=ORIENTED_EDGE('',*,*,#2394,.T.);
#3334=ORIENTED_EDGE('',*,*,#2395,.T.);
#3335=ORIENTED_EDGE('',*,*,#2396,.T.);
#3336=ORIENTED_EDGE('',*,*,#2397,.T.);
#3337=ORIENTED_EDGE('',*,*,#2378,.T.);
#3338=ORIENTED_EDGE('',*,*,#2375,.T.);
#3339=ORIENTED_EDGE('',*,*,#2398,.F.);
#3340=ORIENTED_EDGE('',*,*,#2399,.F.);
#3341=ORIENTED_EDGE('',*,*,#2379,.F.);
#3342=ORIENTED_EDGE('',*,*,#2397,.F.);
#3343=ORIENTED_EDGE('',*,*,#2399,.T.);
#3344=ORIENTED_EDGE('',*,*,#2400,.T.);
#3345=ORIENTED_EDGE('',*,*,#2401,.T.);
#3346=ORIENTED_EDGE('',*,*,#2380,.T.);
#3347=ORIENTED_EDGE('',*,*,#2402,.F.);
#3348=ORIENTED_EDGE('',*,*,#2403,.F.);
#3349=ORIENTED_EDGE('',*,*,#2381,.F.);
#3350=ORIENTED_EDGE('',*,*,#2401,.F.);
#3351=ORIENTED_EDGE('',*,*,#2403,.T.);
#3352=ORIENTED_EDGE('',*,*,#2404,.T.);
#3353=ORIENTED_EDGE('',*,*,#2405,.T.);
#3354=ORIENTED_EDGE('',*,*,#2382,.T.);
#3355=ORIENTED_EDGE('',*,*,#2383,.F.);
#3356=ORIENTED_EDGE('',*,*,#2405,.F.);
#3357=ORIENTED_EDGE('',*,*,#2406,.F.);
#3358=ORIENTED_EDGE('',*,*,#2407,.F.);
#3359=ORIENTED_EDGE('',*,*,#2408,.F.);
#3360=ORIENTED_EDGE('',*,*,#2409,.T.);
#3361=ORIENTED_EDGE('',*,*,#2395,.F.);
#3362=ORIENTED_EDGE('',*,*,#2393,.T.);
#3363=ORIENTED_EDGE('',*,*,#2391,.F.);
#3364=ORIENTED_EDGE('',*,*,#2389,.T.);
#3365=ORIENTED_EDGE('',*,*,#2387,.F.);
#3366=ORIENTED_EDGE('',*,*,#2367,.T.);
#3367=ORIENTED_EDGE('',*,*,#2410,.F.);
#3368=ORIENTED_EDGE('',*,*,#2411,.T.);
#3369=ORIENTED_EDGE('',*,*,#2412,.F.);
#3370=ORIENTED_EDGE('',*,*,#2406,.T.);
#3371=ORIENTED_EDGE('',*,*,#2404,.F.);
#3372=ORIENTED_EDGE('',*,*,#2402,.T.);
#3373=ORIENTED_EDGE('',*,*,#2400,.F.);
#3374=ORIENTED_EDGE('',*,*,#2398,.T.);
#3375=ORIENTED_EDGE('',*,*,#2396,.F.);
#3376=ORIENTED_EDGE('',*,*,#2409,.F.);
#3377=ORIENTED_EDGE('',*,*,#2370,.T.);
#3378=ORIENTED_EDGE('',*,*,#2386,.T.);
#3379=ORIENTED_EDGE('',*,*,#2413,.T.);
#3380=ORIENTED_EDGE('',*,*,#2410,.T.);
#3381=ORIENTED_EDGE('',*,*,#2385,.F.);
#3382=ORIENTED_EDGE('',*,*,#2414,.F.);
#3383=ORIENTED_EDGE('',*,*,#2411,.F.);
#3384=ORIENTED_EDGE('',*,*,#2413,.F.);
#3385=ORIENTED_EDGE('',*,*,#2377,.T.);
#3386=ORIENTED_EDGE('',*,*,#2408,.T.);
#3387=ORIENTED_EDGE('',*,*,#2407,.T.);
#3388=ORIENTED_EDGE('',*,*,#2412,.T.);
#3389=ORIENTED_EDGE('',*,*,#2414,.T.);
#3390=ORIENTED_EDGE('',*,*,#2384,.T.);
#3391=ORIENTED_EDGE('',*,*,#2415,.F.);
#3392=ORIENTED_EDGE('',*,*,#2416,.T.);
#3393=ORIENTED_EDGE('',*,*,#2417,.F.);
#3394=ORIENTED_EDGE('',*,*,#2418,.T.);
#3395=ORIENTED_EDGE('',*,*,#2415,.T.);
#3396=ORIENTED_EDGE('',*,*,#2418,.F.);
#3397=ORIENTED_EDGE('',*,*,#2417,.T.);
#3398=ORIENTED_EDGE('',*,*,#2419,.F.);
#3399=ORIENTED_EDGE('',*,*,#2419,.T.);
#3400=ORIENTED_EDGE('',*,*,#2420,.T.);
#3401=ORIENTED_EDGE('',*,*,#2416,.F.);
#3402=ORIENTED_EDGE('',*,*,#2420,.F.);
#3403=ORIENTED_EDGE('',*,*,#2421,.F.);
#3404=ORIENTED_EDGE('',*,*,#2422,.T.);
#3405=ORIENTED_EDGE('',*,*,#2423,.F.);
#3406=ORIENTED_EDGE('',*,*,#2424,.T.);
#3407=ORIENTED_EDGE('',*,*,#2421,.T.);
#3408=ORIENTED_EDGE('',*,*,#2424,.F.);
#3409=ORIENTED_EDGE('',*,*,#2423,.T.);
#3410=ORIENTED_EDGE('',*,*,#2425,.F.);
#3411=ORIENTED_EDGE('',*,*,#2425,.T.);
#3412=ORIENTED_EDGE('',*,*,#2426,.T.);
#3413=ORIENTED_EDGE('',*,*,#2422,.F.);
#3414=ORIENTED_EDGE('',*,*,#2426,.F.);
#3415=ORIENTED_EDGE('',*,*,#2427,.F.);
#3416=ORIENTED_EDGE('',*,*,#2428,.T.);
#3417=ORIENTED_EDGE('',*,*,#2429,.T.);
#3418=ORIENTED_EDGE('',*,*,#2428,.F.);
#3419=ORIENTED_EDGE('',*,*,#2430,.F.);
#3420=ORIENTED_EDGE('',*,*,#2431,.T.);
#3421=ORIENTED_EDGE('',*,*,#2432,.T.);
#3422=ORIENTED_EDGE('',*,*,#2431,.F.);
#3423=ORIENTED_EDGE('',*,*,#2430,.T.);
#3424=ORIENTED_EDGE('',*,*,#2427,.T.);
#3425=ORIENTED_EDGE('',*,*,#2432,.F.);
#3426=ORIENTED_EDGE('',*,*,#2429,.F.);
#3427=CYLINDRICAL_SURFACE('',#3965,0.75);
#3428=CYLINDRICAL_SURFACE('',#3968,0.425);
#3429=CYLINDRICAL_SURFACE('',#3971,0.425);
#3430=CYLINDRICAL_SURFACE('',#3974,0.425);
#3431=CYLINDRICAL_SURFACE('',#3977,0.425);
#3432=CYLINDRICAL_SURFACE('',#3987,0.4);
#3433=CYLINDRICAL_SURFACE('',#3994,1.2);
#3434=CYLINDRICAL_SURFACE('',#4000,0.75);
#3435=CYLINDRICAL_SURFACE('',#4001,0.6);
#3436=CYLINDRICAL_SURFACE('',#4006,0.22);
#3437=CYLINDRICAL_SURFACE('',#4010,0.22);
#3438=CYLINDRICAL_SURFACE('',#4015,0.22);
#3439=CYLINDRICAL_SURFACE('',#4020,0.22);
#3440=CYLINDRICAL_SURFACE('',#4024,0.22);
#3441=CYLINDRICAL_SURFACE('',#4028,0.22);
#3442=CYLINDRICAL_SURFACE('',#4032,0.22);
#3443=CYLINDRICAL_SURFACE('',#4037,0.22);
#3444=CYLINDRICAL_SURFACE('',#4042,0.22);
#3445=CYLINDRICAL_SURFACE('',#4046,0.22);
#3446=CYLINDRICAL_SURFACE('',#4084,1.4);
#3447=CYLINDRICAL_SURFACE('',#4088,0.75);
#3448=CYLINDRICAL_SURFACE('',#4090,0.22);
#3449=CYLINDRICAL_SURFACE('',#4094,0.22);
#3450=CYLINDRICAL_SURFACE('',#4099,0.22);
#3451=CYLINDRICAL_SURFACE('',#4104,0.22);
#3452=CYLINDRICAL_SURFACE('',#4108,0.22);
#3453=CYLINDRICAL_SURFACE('',#4112,0.22);
#3454=CYLINDRICAL_SURFACE('',#4116,0.22);
#3455=CYLINDRICAL_SURFACE('',#4121,0.22);
#3456=CYLINDRICAL_SURFACE('',#4126,0.22);
#3457=CYLINDRICAL_SURFACE('',#4130,0.22);
#3458=CYLINDRICAL_SURFACE('',#4169,1.4);
#3459=CYLINDRICAL_SURFACE('',#4172,0.8);
#3460=CYLINDRICAL_SURFACE('',#4198,0.42);
#3461=CYLINDRICAL_SURFACE('',#4201,0.8);
#3462=CYLINDRICAL_SURFACE('',#4214,0.338975);
#3463=CYLINDRICAL_SURFACE('',#4229,0.8);
#3464=CYLINDRICAL_SURFACE('',#4232,0.6);
#3465=CYLINDRICAL_SURFACE('',#4235,0.6);
#3466=CYLINDRICAL_SURFACE('',#4255,0.605);
#3467=CYLINDRICAL_SURFACE('',#4258,0.8);
#3468=CYLINDRICAL_SURFACE('',#4264,0.165);
#3469=CYLINDRICAL_SURFACE('',#4271,0.9);
#3470=CYLINDRICAL_SURFACE('',#4274,0.6);
#3471=CYLINDRICAL_SURFACE('',#4278,0.605);
#3472=CYLINDRICAL_SURFACE('',#4281,0.8);
#3473=CYLINDRICAL_SURFACE('',#4287,0.225);
#3474=CYLINDRICAL_SURFACE('',#4290,0.8);
#3475=CYLINDRICAL_SURFACE('',#4310,0.35);
#3476=CYLINDRICAL_SURFACE('',#4318,0.1954);
#3477=CYLINDRICAL_SURFACE('',#4328,1.6);
#3478=CYLINDRICAL_SURFACE('',#4333,1.6);
#3479=CYLINDRICAL_SURFACE('',#4338,0.62);
#3480=CYLINDRICAL_SURFACE('',#4339,3.75);
#3481=CYLINDRICAL_SURFACE('',#4352,1.070235);
#3482=CYLINDRICAL_SURFACE('',#4354,0.6);
#3483=CYLINDRICAL_SURFACE('',#4360,1.070235);
#3484=CYLINDRICAL_SURFACE('',#4372,1.129765);
#3485=CYLINDRICAL_SURFACE('',#4379,1.6);
#3486=CYLINDRICAL_SURFACE('',#4384,1.129765);
#3487=CYLINDRICAL_SURFACE('',#4404,1.123812);
#3488=CYLINDRICAL_SURFACE('',#4440,1.076188);
#3489=CYLINDRICAL_SURFACE('',#4454,1.119765);
#3490=CYLINDRICAL_SURFACE('',#4458,1.085235);
#3491=CYLINDRICAL_SURFACE('',#4462,1.119765);
#3492=CYLINDRICAL_SURFACE('',#4466,1.085235);
#3493=CYLINDRICAL_SURFACE('',#4473,1.2);
#3494=CYLINDRICAL_SURFACE('',#4476,1.6);
#3495=ADVANCED_FACE('',(#524),#3427,.F.);
#3496=ADVANCED_FACE('',(#525),#3428,.F.);
#3497=ADVANCED_FACE('',(#526),#3429,.F.);
#3498=ADVANCED_FACE('',(#527),#3430,.F.);
#3499=ADVANCED_FACE('',(#528),#3431,.F.);
#3500=ADVANCED_FACE('',(#529),#438,.T.);
#3501=ADVANCED_FACE('',(#530),#439,.T.);
#3502=ADVANCED_FACE('',(#531),#440,.T.);
#3503=ADVANCED_FACE('',(#532),#441,.T.);
#3504=ADVANCED_FACE('',(#533,#369,#370,#371,#372,#373),#442,.T.);
#3505=ADVANCED_FACE('',(#534,#374,#375,#376,#377,#378),#443,.F.);
#3506=ADVANCED_FACE('',(#535),#3432,.T.);
#3507=ADVANCED_FACE('',(#536),#444,.F.);
#3508=ADVANCED_FACE('',(#537,#379),#445,.F.);
#3509=ADVANCED_FACE('',(#538),#3433,.T.);
#3510=ADVANCED_FACE('',(#539),#446,.T.);
#3511=ADVANCED_FACE('',(#540,#380),#447,.F.);
#3512=ADVANCED_FACE('',(#541),#3434,.T.);
#3513=ADVANCED_FACE('',(#542),#3435,.T.);
#3514=ADVANCED_FACE('',(#543,#381),#448,.F.);
#3515=ADVANCED_FACE('',(#544),#3436,.F.);
#3516=ADVANCED_FACE('',(#545),#3437,.F.);
#3517=ADVANCED_FACE('',(#546),#3438,.F.);
#3518=ADVANCED_FACE('',(#547),#3439,.F.);
#3519=ADVANCED_FACE('',(#548),#3440,.F.);
#3520=ADVANCED_FACE('',(#549),#3441,.F.);
#3521=ADVANCED_FACE('',(#550),#3442,.F.);
#3522=ADVANCED_FACE('',(#551),#3443,.F.);
#3523=ADVANCED_FACE('',(#552),#3444,.F.);
#3524=ADVANCED_FACE('',(#553),#3445,.F.);
#3525=ADVANCED_FACE('',(#554,#382),#449,.T.);
#3526=ADVANCED_FACE('',(#555),#170,.F.);
#3527=ADVANCED_FACE('',(#556),#171,.F.);
#3528=ADVANCED_FACE('',(#557),#172,.F.);
#3529=ADVANCED_FACE('',(#558),#173,.F.);
#3530=ADVANCED_FACE('',(#559),#174,.F.);
#3531=ADVANCED_FACE('',(#560),#175,.F.);
#3532=ADVANCED_FACE('',(#561),#176,.F.);
#3533=ADVANCED_FACE('',(#562),#177,.F.);
#3534=ADVANCED_FACE('',(#563),#178,.F.);
#3535=ADVANCED_FACE('',(#564),#179,.F.);
#3536=ADVANCED_FACE('',(#565,#383),#450,.T.);
#3537=ADVANCED_FACE('',(#566),#3446,.T.);
#3538=ADVANCED_FACE('',(#567,#384,#385,#386,#387,#388,#389,#390,#391,#392,
#393,#394),#451,.T.);
#3539=ADVANCED_FACE('',(#568),#3447,.F.);
#3540=ADVANCED_FACE('',(#569),#3448,.F.);
#3541=ADVANCED_FACE('',(#570),#3449,.F.);
#3542=ADVANCED_FACE('',(#571),#3450,.F.);
#3543=ADVANCED_FACE('',(#572),#3451,.F.);
#3544=ADVANCED_FACE('',(#573),#3452,.F.);
#3545=ADVANCED_FACE('',(#574),#3453,.F.);
#3546=ADVANCED_FACE('',(#575),#3454,.F.);
#3547=ADVANCED_FACE('',(#576),#3455,.F.);
#3548=ADVANCED_FACE('',(#577),#3456,.F.);
#3549=ADVANCED_FACE('',(#578),#3457,.F.);
#3550=ADVANCED_FACE('',(#579,#395),#452,.T.);
#3551=ADVANCED_FACE('',(#580),#180,.F.);
#3552=ADVANCED_FACE('',(#581),#181,.F.);
#3553=ADVANCED_FACE('',(#582),#182,.F.);
#3554=ADVANCED_FACE('',(#583),#183,.F.);
#3555=ADVANCED_FACE('',(#584),#184,.F.);
#3556=ADVANCED_FACE('',(#585),#185,.F.);
#3557=ADVANCED_FACE('',(#586),#186,.F.);
#3558=ADVANCED_FACE('',(#587),#187,.F.);
#3559=ADVANCED_FACE('',(#588),#188,.F.);
#3560=ADVANCED_FACE('',(#589),#189,.F.);
#3561=ADVANCED_FACE('',(#590,#396,#397,#398,#399,#400,#401,#402,#403,#404,
#405,#406),#453,.T.);
#3562=ADVANCED_FACE('',(#591),#3458,.T.);
#3563=ADVANCED_FACE('',(#592,#407),#454,.T.);
#3564=ADVANCED_FACE('',(#593),#3459,.F.);
#3565=ADVANCED_FACE('',(#594),#146,.T.);
#3566=ADVANCED_FACE('',(#595),#147,.T.);
#3567=ADVANCED_FACE('',(#596),#148,.T.);
#3568=ADVANCED_FACE('',(#597),#149,.T.);
#3569=ADVANCED_FACE('',(#598),#150,.T.);
#3570=ADVANCED_FACE('',(#599),#151,.T.);
#3571=ADVANCED_FACE('',(#600),#152,.T.);
#3572=ADVANCED_FACE('',(#601),#153,.T.);
#3573=ADVANCED_FACE('',(#602),#154,.T.);
#3574=ADVANCED_FACE('',(#603),#155,.T.);
#3575=ADVANCED_FACE('',(#604),#3460,.F.);
#3576=ADVANCED_FACE('',(#605),#3461,.T.);
#3577=ADVANCED_FACE('',(#606,#408),#455,.T.);
#3578=ADVANCED_FACE('',(#607,#409),#456,.F.);
#3579=ADVANCED_FACE('',(#608),#25,.T.);
#3580=ADVANCED_FACE('',(#609),#26,.T.);
#3581=ADVANCED_FACE('',(#610),#457,.T.);
#3582=ADVANCED_FACE('',(#611),#458,.T.);
#3583=ADVANCED_FACE('',(#612),#459,.T.);
#3584=ADVANCED_FACE('',(#613),#3462,.F.);
#3585=ADVANCED_FACE('',(#614),#460,.T.);
#3586=ADVANCED_FACE('',(#615),#461,.T.);
#3587=ADVANCED_FACE('',(#616),#462,.T.);
#3588=ADVANCED_FACE('',(#617,#410),#463,.T.);
#3589=ADVANCED_FACE('',(#618,#411),#464,.F.);
#3590=ADVANCED_FACE('',(#619),#3463,.F.);
#3591=ADVANCED_FACE('',(#620),#3464,.F.);
#3592=ADVANCED_FACE('',(#621),#3465,.F.);
#3593=ADVANCED_FACE('',(#622),#465,.T.);
#3594=ADVANCED_FACE('',(#623),#466,.T.);
#3595=ADVANCED_FACE('',(#624),#467,.T.);
#3596=ADVANCED_FACE('',(#625),#468,.T.);
#3597=ADVANCED_FACE('',(#626),#469,.T.);
#3598=ADVANCED_FACE('',(#627),#470,.T.);
#3599=ADVANCED_FACE('',(#628),#471,.T.);
#3600=ADVANCED_FACE('',(#629),#472,.F.);
#3601=ADVANCED_FACE('',(#630,#412),#473,.F.);
#3602=ADVANCED_FACE('',(#631),#474,.T.);
#3603=ADVANCED_FACE('',(#632),#475,.T.);
#3604=ADVANCED_FACE('',(#633),#476,.T.);
#3605=ADVANCED_FACE('',(#634),#477,.T.);
#3606=ADVANCED_FACE('',(#635),#478,.T.);
#3607=ADVANCED_FACE('',(#636),#479,.T.);
#3608=ADVANCED_FACE('',(#637,#413),#480,.T.);
#3609=ADVANCED_FACE('',(#638),#3466,.F.);
#3610=ADVANCED_FACE('',(#639),#3467,.T.);
#3611=ADVANCED_FACE('',(#640,#414),#481,.T.);
#3612=ADVANCED_FACE('',(#641,#415),#482,.F.);
#3613=ADVANCED_FACE('',(#642),#3468,.F.);
#3614=ADVANCED_FACE('',(#643),#483,.T.);
#3615=ADVANCED_FACE('',(#644,#416),#484,.T.);
#3616=ADVANCED_FACE('',(#645),#3469,.T.);
#3617=ADVANCED_FACE('',(#646),#485,.F.);
#3618=ADVANCED_FACE('',(#647),#3470,.T.);
#3619=ADVANCED_FACE('',(#648,#417),#486,.T.);
#3620=ADVANCED_FACE('',(#649),#3471,.F.);
#3621=ADVANCED_FACE('',(#650),#3472,.T.);
#3622=ADVANCED_FACE('',(#651,#418),#487,.T.);
#3623=ADVANCED_FACE('',(#652,#419),#488,.F.);
#3624=ADVANCED_FACE('',(#653),#3473,.F.);
#3625=ADVANCED_FACE('',(#654),#3474,.T.);
#3626=ADVANCED_FACE('',(#655,#420),#489,.T.);
#3627=ADVANCED_FACE('',(#656,#421),#490,.F.);
#3628=ADVANCED_FACE('',(#657),#491,.F.);
#3629=ADVANCED_FACE('',(#658),#492,.F.);
#3630=ADVANCED_FACE('',(#659),#493,.F.);
#3631=ADVANCED_FACE('',(#660),#494,.F.);
#3632=ADVANCED_FACE('',(#661),#495,.F.);
#3633=ADVANCED_FACE('',(#662),#496,.F.);
#3634=ADVANCED_FACE('',(#663),#497,.F.);
#3635=ADVANCED_FACE('',(#664),#498,.F.);
#3636=ADVANCED_FACE('',(#665),#499,.F.);
#3637=ADVANCED_FACE('',(#666),#500,.T.);
#3638=ADVANCED_FACE('',(#667),#27,.T.);
#3639=ADVANCED_FACE('',(#668),#3475,.T.);
#3640=ADVANCED_FACE('',(#669),#28,.T.);
#3641=ADVANCED_FACE('',(#670,#422),#501,.T.);
#3642=ADVANCED_FACE('',(#671),#29,.T.);
#3643=ADVANCED_FACE('',(#672),#3476,.T.);
#3644=ADVANCED_FACE('',(#673),#3477,.F.);
#3645=ADVANCED_FACE('',(#674,#423),#502,.T.);
#3646=ADVANCED_FACE('',(#675),#3478,.F.);
#3647=ADVANCED_FACE('',(#676,#424),#503,.F.);
#3648=ADVANCED_FACE('',(#677),#3479,.F.);
#3649=ADVANCED_FACE('',(#678),#3480,.T.);
#3650=ADVANCED_FACE('',(#679,#425),#504,.T.);
#3651=ADVANCED_FACE('',(#680,#426),#505,.F.);
#3652=ADVANCED_FACE('',(#681),#190,.F.);
#3653=ADVANCED_FACE('',(#682),#3481,.T.);
#3654=ADVANCED_FACE('',(#683),#3482,.F.);
#3655=ADVANCED_FACE('',(#684),#30,.F.);
#3656=ADVANCED_FACE('',(#685,#427),#506,.T.);
#3657=ADVANCED_FACE('',(#686),#3483,.T.);
#3658=ADVANCED_FACE('',(#687,#428),#507,.T.);
#3659=ADVANCED_FACE('',(#688),#31,.F.);
#3660=ADVANCED_FACE('',(#689),#191,.F.);
#3661=ADVANCED_FACE('',(#690),#3484,.F.);
#3662=ADVANCED_FACE('',(#691,#429),#508,.T.);
#3663=ADVANCED_FACE('',(#692),#32,.T.);
#3664=ADVANCED_FACE('',(#693),#3485,.T.);
#3665=ADVANCED_FACE('',(#694),#33,.T.);
#3666=ADVANCED_FACE('',(#695,#430),#509,.T.);
#3667=ADVANCED_FACE('',(#696),#3486,.F.);
#3668=ADVANCED_FACE('',(#697),#156,.T.);
#3669=ADVANCED_FACE('',(#698),#157,.T.);
#3670=ADVANCED_FACE('',(#699),#158,.T.);
#3671=ADVANCED_FACE('',(#700),#159,.T.);
#3672=ADVANCED_FACE('',(#701),#160,.T.);
#3673=ADVANCED_FACE('',(#702),#161,.T.);
#3674=ADVANCED_FACE('',(#703),#162,.T.);
#3675=ADVANCED_FACE('',(#704),#163,.F.);
#3676=ADVANCED_FACE('',(#705),#3487,.T.);
#3677=ADVANCED_FACE('',(#706),#510,.T.);
#3678=ADVANCED_FACE('',(#707),#164,.F.);
#3679=ADVANCED_FACE('',(#708),#511,.T.);
#3680=ADVANCED_FACE('',(#709),#165,.F.);
#3681=ADVANCED_FACE('',(#710),#512,.T.);
#3682=ADVANCED_FACE('',(#711),#166,.F.);
#3683=ADVANCED_FACE('',(#712),#513,.T.);
#3684=ADVANCED_FACE('',(#713),#167,.F.);
#3685=ADVANCED_FACE('',(#714),#514,.T.);
#3686=ADVANCED_FACE('',(#715),#168,.F.);
#3687=ADVANCED_FACE('',(#716),#3488,.F.);
#3688=ADVANCED_FACE('',(#717),#515,.T.);
#3689=ADVANCED_FACE('',(#718),#169,.F.);
#3690=ADVANCED_FACE('',(#719,#431),#516,.T.);
#3691=ADVANCED_FACE('',(#720),#517,.T.);
#3692=ADVANCED_FACE('',(#721,#432),#518,.T.);
#3693=ADVANCED_FACE('',(#722),#3489,.T.);
#3694=ADVANCED_FACE('',(#723,#433),#519,.T.);
#3695=ADVANCED_FACE('',(#724),#3490,.F.);
#3696=ADVANCED_FACE('',(#725,#434),#520,.T.);
#3697=ADVANCED_FACE('',(#726),#3491,.T.);
#3698=ADVANCED_FACE('',(#727,#435),#521,.T.);
#3699=ADVANCED_FACE('',(#728),#3492,.F.);
#3700=ADVANCED_FACE('',(#729),#3493,.F.);
#3701=ADVANCED_FACE('',(#730),#3494,.T.);
#3702=ADVANCED_FACE('',(#731,#436),#522,.T.);
#3703=ADVANCED_FACE('',(#732,#437),#523,.F.);
#3704=CLOSED_SHELL('',(#3495,#3496,#3497,#3498,#3499,#3500,#3501,#3502,
#3503,#3504,#3505));
#3705=CLOSED_SHELL('',(#3506,#3507,#3508,#3509,#3510,#3511,#3512,#3513,
#3514));
#3706=CLOSED_SHELL('',(#3515,#3516,#3517,#3518,#3519,#3520,#3521,#3522,
#3523,#3524,#3525,#3526,#3527,#3528,#3529,#3530,#3531,#3532,#3533,#3534,
#3535,#3536,#3537,#3538,#3539));
#3707=CLOSED_SHELL('',(#3540,#3541,#3542,#3543,#3544,#3545,#3546,#3547,
#3548,#3549,#3550,#3551,#3552,#3553,#3554,#3555,#3556,#3557,#3558,#3559,
#3560,#3561,#3562,#3563,#3564));
#3708=CLOSED_SHELL('',(#3565));
#3709=CLOSED_SHELL('',(#3566));
#3710=CLOSED_SHELL('',(#3567));
#3711=CLOSED_SHELL('',(#3568));
#3712=CLOSED_SHELL('',(#3569));
#3713=CLOSED_SHELL('',(#3570));
#3714=CLOSED_SHELL('',(#3571));
#3715=CLOSED_SHELL('',(#3572));
#3716=CLOSED_SHELL('',(#3573));
#3717=CLOSED_SHELL('',(#3574));
#3718=CLOSED_SHELL('',(#3575,#3576,#3577,#3578));
#3719=CLOSED_SHELL('',(#3579,#3580,#3581,#3582,#3583,#3584,#3585,#3586,
#3587,#3588,#3589));
#3720=CLOSED_SHELL('',(#3590,#3591,#3592,#3593,#3594,#3595,#3596,#3597,
#3598,#3599,#3600,#3601,#3602,#3603,#3604,#3605,#3606,#3607,#3608));
#3721=CLOSED_SHELL('',(#3609,#3610,#3611,#3612));
#3722=CLOSED_SHELL('',(#3613,#3614,#3615,#3616,#3617,#3618,#3619));
#3723=CLOSED_SHELL('',(#3620,#3621,#3622,#3623));
#3724=CLOSED_SHELL('',(#3624,#3625,#3626,#3627));
#3725=CLOSED_SHELL('',(#3628,#3629,#3630,#3631,#3632,#3633,#3634,#3635));
#3726=CLOSED_SHELL('',(#3636,#3637,#3638,#3639,#3640,#3641,#3642,#3643));
#3727=CLOSED_SHELL('',(#3644,#3645,#3646,#3647,#3648,#3649,#3650,#3651));
#3728=CLOSED_SHELL('',(#3652,#3653,#3654,#3655,#3656,#3657,#3658,#3659));
#3729=CLOSED_SHELL('',(#3660,#3661,#3662,#3663,#3664,#3665,#3666,#3667));
#3730=CLOSED_SHELL('',(#3668));
#3731=CLOSED_SHELL('',(#3669));
#3732=CLOSED_SHELL('',(#3670));
#3733=CLOSED_SHELL('',(#3671));
#3734=CLOSED_SHELL('',(#3672));
#3735=CLOSED_SHELL('',(#3673));
#3736=CLOSED_SHELL('',(#3674));
#3737=CLOSED_SHELL('',(#3675,#3676,#3677,#3678,#3679,#3680,#3681,#3682,
#3683,#3684,#3685,#3686,#3687,#3688,#3689,#3690,#3691));
#3738=CLOSED_SHELL('',(#3692,#3693,#3694,#3695));
#3739=CLOSED_SHELL('',(#3696,#3697,#3698,#3699));
#3740=CLOSED_SHELL('',(#3700,#3701,#3702,#3703));
#3741=DERIVED_UNIT_ELEMENT(#3781,1.);
#3742=DERIVED_UNIT_ELEMENT(#7818,-3.);
#3743=DERIVED_UNIT_ELEMENT(#3781,1.);
#3744=DERIVED_UNIT_ELEMENT(#7818,-3.);
#3745=DERIVED_UNIT_ELEMENT(#3781,1.);
#3746=DERIVED_UNIT_ELEMENT(#7818,-3.);
#3747=DERIVED_UNIT_ELEMENT(#3781,1.);
#3748=DERIVED_UNIT_ELEMENT(#7818,-3.);
#3749=DERIVED_UNIT_ELEMENT(#3781,1.);
#3750=DERIVED_UNIT_ELEMENT(#7818,-3.);
#3751=DERIVED_UNIT_ELEMENT(#3781,1.);
#3752=DERIVED_UNIT_ELEMENT(#7818,-3.);
#3753=DERIVED_UNIT_ELEMENT(#3781,1.);
#3754=DERIVED_UNIT_ELEMENT(#7818,-3.);
#3755=DERIVED_UNIT_ELEMENT(#3781,1.);
#3756=DERIVED_UNIT_ELEMENT(#7818,-3.);
#3757=DERIVED_UNIT_ELEMENT(#3781,1.);
#3758=DERIVED_UNIT_ELEMENT(#7818,-3.);
#3759=DERIVED_UNIT_ELEMENT(#3781,1.);
#3760=DERIVED_UNIT_ELEMENT(#7818,-3.);
#3761=DERIVED_UNIT_ELEMENT(#3781,1.);
#3762=DERIVED_UNIT_ELEMENT(#7818,-3.);
#3763=DERIVED_UNIT_ELEMENT(#3781,1.);
#3764=DERIVED_UNIT_ELEMENT(#7818,-3.);
#3765=DERIVED_UNIT_ELEMENT(#3781,1.);
#3766=DERIVED_UNIT_ELEMENT(#7818,-3.);
#3767=DERIVED_UNIT_ELEMENT(#3781,1.);
#3768=DERIVED_UNIT_ELEMENT(#7818,-3.);
#3769=DERIVED_UNIT_ELEMENT(#3781,1.);
#3770=DERIVED_UNIT_ELEMENT(#7818,-3.);
#3771=DERIVED_UNIT_ELEMENT(#3781,1.);
#3772=DERIVED_UNIT_ELEMENT(#7818,-3.);
#3773=DERIVED_UNIT_ELEMENT(#3781,1.);
#3774=DERIVED_UNIT_ELEMENT(#7818,-3.);
#3775=DERIVED_UNIT_ELEMENT(#3781,1.);
#3776=DERIVED_UNIT_ELEMENT(#7818,-3.);
#3777=DERIVED_UNIT_ELEMENT(#3781,1.);
#3778=DERIVED_UNIT_ELEMENT(#7818,-3.);
#3779=DERIVED_UNIT_ELEMENT(#3781,1.);
#3780=DERIVED_UNIT_ELEMENT(#7818,-3.);
#3781=(
MASS_UNIT()
NAMED_UNIT(*)
SI_UNIT(.KILO.,.GRAM.)
);
#3782=DERIVED_UNIT((#3741,#3742));
#3783=DERIVED_UNIT((#3743,#3744));
#3784=DERIVED_UNIT((#3745,#3746));
#3785=DERIVED_UNIT((#3747,#3748));
#3786=DERIVED_UNIT((#3749,#3750));
#3787=DERIVED_UNIT((#3751,#3752));
#3788=DERIVED_UNIT((#3753,#3754));
#3789=DERIVED_UNIT((#3755,#3756));
#3790=DERIVED_UNIT((#3757,#3758));
#3791=DERIVED_UNIT((#3759,#3760));
#3792=DERIVED_UNIT((#3761,#3762));
#3793=DERIVED_UNIT((#3763,#3764));
#3794=DERIVED_UNIT((#3765,#3766));
#3795=DERIVED_UNIT((#3767,#3768));
#3796=DERIVED_UNIT((#3769,#3770));
#3797=DERIVED_UNIT((#3771,#3772));
#3798=DERIVED_UNIT((#3773,#3774));
#3799=DERIVED_UNIT((#3775,#3776));
#3800=DERIVED_UNIT((#3777,#3778));
#3801=DERIVED_UNIT((#3779,#3780));
#3802=MEASURE_REPRESENTATION_ITEM('density measure',
POSITIVE_RATIO_MEASURE(7850.),#3782);
#3803=MEASURE_REPRESENTATION_ITEM('density measure',
POSITIVE_RATIO_MEASURE(7850.),#3783);
#3804=MEASURE_REPRESENTATION_ITEM('density measure',
POSITIVE_RATIO_MEASURE(7850.),#3784);
#3805=MEASURE_REPRESENTATION_ITEM('density measure',
POSITIVE_RATIO_MEASURE(7850.),#3785);
#3806=MEASURE_REPRESENTATION_ITEM('density measure',
POSITIVE_RATIO_MEASURE(7850.),#3786);
#3807=MEASURE_REPRESENTATION_ITEM('density measure',
POSITIVE_RATIO_MEASURE(7850.),#3787);
#3808=MEASURE_REPRESENTATION_ITEM('density measure',
POSITIVE_RATIO_MEASURE(7850.),#3788);
#3809=MEASURE_REPRESENTATION_ITEM('density measure',
POSITIVE_RATIO_MEASURE(7850.),#3789);
#3810=MEASURE_REPRESENTATION_ITEM('density measure',
POSITIVE_RATIO_MEASURE(7850.),#3790);
#3811=MEASURE_REPRESENTATION_ITEM('density measure',
POSITIVE_RATIO_MEASURE(7850.),#3791);
#3812=MEASURE_REPRESENTATION_ITEM('density measure',
POSITIVE_RATIO_MEASURE(7850.),#3792);
#3813=MEASURE_REPRESENTATION_ITEM('density measure',
POSITIVE_RATIO_MEASURE(7850.),#3793);
#3814=MEASURE_REPRESENTATION_ITEM('density measure',
POSITIVE_RATIO_MEASURE(7850.),#3794);
#3815=MEASURE_REPRESENTATION_ITEM('density measure',
POSITIVE_RATIO_MEASURE(7850.),#3795);
#3816=MEASURE_REPRESENTATION_ITEM('density measure',
POSITIVE_RATIO_MEASURE(7850.),#3796);
#3817=MEASURE_REPRESENTATION_ITEM('density measure',
POSITIVE_RATIO_MEASURE(7850.),#3797);
#3818=MEASURE_REPRESENTATION_ITEM('density measure',
POSITIVE_RATIO_MEASURE(7850.),#3798);
#3819=MEASURE_REPRESENTATION_ITEM('density measure',
POSITIVE_RATIO_MEASURE(7850.),#3799);
#3820=MEASURE_REPRESENTATION_ITEM('density measure',
POSITIVE_RATIO_MEASURE(7850.),#3800);
#3821=MEASURE_REPRESENTATION_ITEM('density measure',
POSITIVE_RATIO_MEASURE(7850.),#3801);
#3822=PROPERTY_DEFINITION_REPRESENTATION(#3922,#3862);
#3823=PROPERTY_DEFINITION_REPRESENTATION(#3923,#3863);
#3824=PROPERTY_DEFINITION_REPRESENTATION(#3924,#3864);
#3825=PROPERTY_DEFINITION_REPRESENTATION(#3925,#3865);
#3826=PROPERTY_DEFINITION_REPRESENTATION(#3926,#3866);
#3827=PROPERTY_DEFINITION_REPRESENTATION(#3927,#3867);
#3828=PROPERTY_DEFINITION_REPRESENTATION(#3928,#3868);
#3829=PROPERTY_DEFINITION_REPRESENTATION(#3929,#3869);
#3830=PROPERTY_DEFINITION_REPRESENTATION(#3930,#3870);
#3831=PROPERTY_DEFINITION_REPRESENTATION(#3931,#3871);
#3832=PROPERTY_DEFINITION_REPRESENTATION(#3932,#3872);
#3833=PROPERTY_DEFINITION_REPRESENTATION(#3933,#3873);
#3834=PROPERTY_DEFINITION_REPRESENTATION(#3934,#3874);
#3835=PROPERTY_DEFINITION_REPRESENTATION(#3935,#3875);
#3836=PROPERTY_DEFINITION_REPRESENTATION(#3936,#3876);
#3837=PROPERTY_DEFINITION_REPRESENTATION(#3937,#3877);
#3838=PROPERTY_DEFINITION_REPRESENTATION(#3938,#3878);
#3839=PROPERTY_DEFINITION_REPRESENTATION(#3939,#3879);
#3840=PROPERTY_DEFINITION_REPRESENTATION(#3940,#3880);
#3841=PROPERTY_DEFINITION_REPRESENTATION(#3941,#3881);
#3842=PROPERTY_DEFINITION_REPRESENTATION(#3942,#3882);
#3843=PROPERTY_DEFINITION_REPRESENTATION(#3943,#3883);
#3844=PROPERTY_DEFINITION_REPRESENTATION(#3944,#3884);
#3845=PROPERTY_DEFINITION_REPRESENTATION(#3945,#3885);
#3846=PROPERTY_DEFINITION_REPRESENTATION(#3946,#3886);
#3847=PROPERTY_DEFINITION_REPRESENTATION(#3947,#3887);
#3848=PROPERTY_DEFINITION_REPRESENTATION(#3948,#3888);
#3849=PROPERTY_DEFINITION_REPRESENTATION(#3949,#3889);
#3850=PROPERTY_DEFINITION_REPRESENTATION(#3950,#3890);
#3851=PROPERTY_DEFINITION_REPRESENTATION(#3951,#3891);
#3852=PROPERTY_DEFINITION_REPRESENTATION(#3952,#3892);
#3853=PROPERTY_DEFINITION_REPRESENTATION(#3953,#3893);
#3854=PROPERTY_DEFINITION_REPRESENTATION(#3954,#3894);
#3855=PROPERTY_DEFINITION_REPRESENTATION(#3955,#3895);
#3856=PROPERTY_DEFINITION_REPRESENTATION(#3956,#3896);
#3857=PROPERTY_DEFINITION_REPRESENTATION(#3957,#3897);
#3858=PROPERTY_DEFINITION_REPRESENTATION(#3958,#3898);
#3859=PROPERTY_DEFINITION_REPRESENTATION(#3959,#3899);
#3860=PROPERTY_DEFINITION_REPRESENTATION(#3960,#3900);
#3861=PROPERTY_DEFINITION_REPRESENTATION(#3961,#3901);
#3862=REPRESENTATION('material name',(#3902),#7792);
#3863=REPRESENTATION('density',(#3802),#7792);
#3864=REPRESENTATION('material name',(#3903),#7793);
#3865=REPRESENTATION('density',(#3803),#7793);
#3866=REPRESENTATION('material name',(#3904),#7795);
#3867=REPRESENTATION('density',(#3804),#7795);
#3868=REPRESENTATION('material name',(#3905),#7796);
#3869=REPRESENTATION('density',(#3805),#7796);
#3870=REPRESENTATION('material name',(#3906),#7797);
#3871=REPRESENTATION('density',(#3806),#7797);
#3872=REPRESENTATION('material name',(#3907),#7798);
#3873=REPRESENTATION('density',(#3807),#7798);
#3874=REPRESENTATION('material name',(#3908),#7799);
#3875=REPRESENTATION('density',(#3808),#7799);
#3876=REPRESENTATION('material name',(#3909),#7801);
#3877=REPRESENTATION('density',(#3809),#7801);
#3878=REPRESENTATION('material name',(#3910),#7802);
#3879=REPRESENTATION('density',(#3810),#7802);
#3880=REPRESENTATION('material name',(#3911),#7803);
#3881=REPRESENTATION('density',(#3811),#7803);
#3882=REPRESENTATION('material name',(#3912),#7804);
#3883=REPRESENTATION('density',(#3812),#7804);
#3884=REPRESENTATION('material name',(#3913),#7805);
#3885=REPRESENTATION('density',(#3813),#7805);
#3886=REPRESENTATION('material name',(#3914),#7806);
#3887=REPRESENTATION('density',(#3814),#7806);
#3888=REPRESENTATION('material name',(#3915),#7808);
#3889=REPRESENTATION('density',(#3815),#7808);
#3890=REPRESENTATION('material name',(#3916),#7810);
#3891=REPRESENTATION('density',(#3816),#7810);
#3892=REPRESENTATION('material name',(#3917),#7811);
#3893=REPRESENTATION('density',(#3817),#7811);
#3894=REPRESENTATION('material name',(#3918),#7812);
#3895=REPRESENTATION('density',(#3818),#7812);
#3896=REPRESENTATION('material name',(#3919),#7813);
#3897=REPRESENTATION('density',(#3819),#7813);
#3898=REPRESENTATION('material name',(#3920),#7814);
#3899=REPRESENTATION('density',(#3820),#7814);
#3900=REPRESENTATION('material name',(#3921),#7815);
#3901=REPRESENTATION('density',(#3821),#7815);
#3902=DESCRIPTIVE_REPRESENTATION_ITEM('Steel','Steel');
#3903=DESCRIPTIVE_REPRESENTATION_ITEM('Steel','Steel');
#3904=DESCRIPTIVE_REPRESENTATION_ITEM('Steel','Steel');
#3905=DESCRIPTIVE_REPRESENTATION_ITEM('Steel','Steel');
#3906=DESCRIPTIVE_REPRESENTATION_ITEM('Steel','Steel');
#3907=DESCRIPTIVE_REPRESENTATION_ITEM('Steel','Steel');
#3908=DESCRIPTIVE_REPRESENTATION_ITEM('Steel','Steel');
#3909=DESCRIPTIVE_REPRESENTATION_ITEM('Steel','Steel');
#3910=DESCRIPTIVE_REPRESENTATION_ITEM('Steel','Steel');
#3911=DESCRIPTIVE_REPRESENTATION_ITEM('Steel','Steel');
#3912=DESCRIPTIVE_REPRESENTATION_ITEM('Steel','Steel');
#3913=DESCRIPTIVE_REPRESENTATION_ITEM('Steel','Steel');
#3914=DESCRIPTIVE_REPRESENTATION_ITEM('Steel','Steel');
#3915=DESCRIPTIVE_REPRESENTATION_ITEM('Steel','Steel');
#3916=DESCRIPTIVE_REPRESENTATION_ITEM('Steel','Steel');
#3917=DESCRIPTIVE_REPRESENTATION_ITEM('Steel','Steel');
#3918=DESCRIPTIVE_REPRESENTATION_ITEM('Steel','Steel');
#3919=DESCRIPTIVE_REPRESENTATION_ITEM('Steel','Steel');
#3920=DESCRIPTIVE_REPRESENTATION_ITEM('Steel','Steel');
#3921=DESCRIPTIVE_REPRESENTATION_ITEM('Steel','Steel');
#3922=PROPERTY_DEFINITION('material property','material name',#7930);
#3923=PROPERTY_DEFINITION('material property','density of part',#7930);
#3924=PROPERTY_DEFINITION('material property','material name',#7931);
#3925=PROPERTY_DEFINITION('material property','density of part',#7931);
#3926=PROPERTY_DEFINITION('material property','material name',#7933);
#3927=PROPERTY_DEFINITION('material property','density of part',#7933);
#3928=PROPERTY_DEFINITION('material property','material name',#7934);
#3929=PROPERTY_DEFINITION('material property','density of part',#7934);
#3930=PROPERTY_DEFINITION('material property','material name',#7935);
#3931=PROPERTY_DEFINITION('material property','density of part',#7935);
#3932=PROPERTY_DEFINITION('material property','material name',#7936);
#3933=PROPERTY_DEFINITION('material property','density of part',#7936);
#3934=PROPERTY_DEFINITION('material property','material name',#7937);
#3935=PROPERTY_DEFINITION('material property','density of part',#7937);
#3936=PROPERTY_DEFINITION('material property','material name',#7939);
#3937=PROPERTY_DEFINITION('material property','density of part',#7939);
#3938=PROPERTY_DEFINITION('material property','material name',#7940);
#3939=PROPERTY_DEFINITION('material property','density of part',#7940);
#3940=PROPERTY_DEFINITION('material property','material name',#7941);
#3941=PROPERTY_DEFINITION('material property','density of part',#7941);
#3942=PROPERTY_DEFINITION('material property','material name',#7942);
#3943=PROPERTY_DEFINITION('material property','density of part',#7942);
#3944=PROPERTY_DEFINITION('material property','material name',#7943);
#3945=PROPERTY_DEFINITION('material property','density of part',#7943);
#3946=PROPERTY_DEFINITION('material property','material name',#7944);
#3947=PROPERTY_DEFINITION('material property','density of part',#7944);
#3948=PROPERTY_DEFINITION('material property','material name',#7946);
#3949=PROPERTY_DEFINITION('material property','density of part',#7946);
#3950=PROPERTY_DEFINITION('material property','material name',#7948);
#3951=PROPERTY_DEFINITION('material property','density of part',#7948);
#3952=PROPERTY_DEFINITION('material property','material name',#7949);
#3953=PROPERTY_DEFINITION('material property','density of part',#7949);
#3954=PROPERTY_DEFINITION('material property','material name',#7950);
#3955=PROPERTY_DEFINITION('material property','density of part',#7950);
#3956=PROPERTY_DEFINITION('material property','material name',#7951);
#3957=PROPERTY_DEFINITION('material property','density of part',#7951);
#3958=PROPERTY_DEFINITION('material property','material name',#7952);
#3959=PROPERTY_DEFINITION('material property','density of part',#7952);
#3960=PROPERTY_DEFINITION('material property','material name',#7953);
#3961=PROPERTY_DEFINITION('material property','density of part',#7953);
#3962=AXIS2_PLACEMENT_3D('',#5698,#4489,#4490);
#3963=AXIS2_PLACEMENT_3D('',#5699,#4491,#4492);
#3964=AXIS2_PLACEMENT_3D('',#5700,#4493,#4494);
#3965=AXIS2_PLACEMENT_3D('',#5701,#4495,#4496);
#3966=AXIS2_PLACEMENT_3D('',#5703,#4497,#4498);
#3967=AXIS2_PLACEMENT_3D('',#5706,#4500,#4501);
#3968=AXIS2_PLACEMENT_3D('',#5707,#4502,#4503);
#3969=AXIS2_PLACEMENT_3D('',#5709,#4504,#4505);
#3970=AXIS2_PLACEMENT_3D('',#5712,#4507,#4508);
#3971=AXIS2_PLACEMENT_3D('',#5713,#4509,#4510);
#3972=AXIS2_PLACEMENT_3D('',#5715,#4511,#4512);
#3973=AXIS2_PLACEMENT_3D('',#5718,#4514,#4515);
#3974=AXIS2_PLACEMENT_3D('',#5719,#4516,#4517);
#3975=AXIS2_PLACEMENT_3D('',#5721,#4518,#4519);
#3976=AXIS2_PLACEMENT_3D('',#5724,#4521,#4522);
#3977=AXIS2_PLACEMENT_3D('',#5725,#4523,#4524);
#3978=AXIS2_PLACEMENT_3D('',#5727,#4525,#4526);
#3979=AXIS2_PLACEMENT_3D('',#5730,#4528,#4529);
#3980=AXIS2_PLACEMENT_3D('',#5731,#4530,#4531);
#3981=AXIS2_PLACEMENT_3D('',#5740,#4536,#4537);
#3982=AXIS2_PLACEMENT_3D('',#5746,#4541,#4542);
#3983=AXIS2_PLACEMENT_3D('',#5752,#4546,#4547);
#3984=AXIS2_PLACEMENT_3D('',#5755,#4550,#4551);
#3985=AXIS2_PLACEMENT_3D('',#5756,#4552,#4553);
#3986=AXIS2_PLACEMENT_3D('',#5757,#4554,#4555);
#3987=AXIS2_PLACEMENT_3D('',#5758,#4556,#4557);
#3988=AXIS2_PLACEMENT_3D('',#5760,#4558,#4559);
#3989=AXIS2_PLACEMENT_3D('',#5763,#4561,#4562);
#3990=AXIS2_PLACEMENT_3D('',#5764,#4563,#4564);
#3991=AXIS2_PLACEMENT_3D('',#5765,#4565,#4566);
#3992=AXIS2_PLACEMENT_3D('',#5767,#4567,#4568);
#3993=AXIS2_PLACEMENT_3D('',#5769,#4569,#4570);
#3994=AXIS2_PLACEMENT_3D('',#5770,#4571,#4572);
#3995=AXIS2_PLACEMENT_3D('',#5772,#4573,#4574);
#3996=AXIS2_PLACEMENT_3D('',#5774,#4576,#4577);
#3997=AXIS2_PLACEMENT_3D('',#5775,#4578,#4579);
#3998=AXIS2_PLACEMENT_3D('',#5777,#4580,#4581);
#3999=AXIS2_PLACEMENT_3D('',#5779,#4582,#4583);
#4000=AXIS2_PLACEMENT_3D('',#5780,#4584,#4585);
#4001=AXIS2_PLACEMENT_3D('',#5782,#4587,#4588);
#4002=AXIS2_PLACEMENT_3D('',#5785,#4590,#4591);
#4003=AXIS2_PLACEMENT_3D('',#5786,#4592,#4593);
#4004=AXIS2_PLACEMENT_3D('',#5787,#4594,#4595);
#4005=AXIS2_PLACEMENT_3D('',#5788,#4596,#4597);
#4006=AXIS2_PLACEMENT_3D('',#5789,#4598,#4599);
#4007=AXIS2_PLACEMENT_3D('',#5791,#4600,#4601);
#4008=AXIS2_PLACEMENT_3D('',#5806,#4603,#4604);
#4009=AXIS2_PLACEMENT_3D('',#5825,#4605,#4606);
#4010=AXIS2_PLACEMENT_3D('',#5836,#4607,#4608);
#4011=AXIS2_PLACEMENT_3D('',#5838,#4609,#4610);
#4012=AXIS2_PLACEMENT_3D('',#5842,#4612,#4613);
#4013=AXIS2_PLACEMENT_3D('',#5861,#4614,#4615);
#4014=AXIS2_PLACEMENT_3D('',#5879,#4616,#4617);
#4015=AXIS2_PLACEMENT_3D('',#5880,#4618,#4619);
#4016=AXIS2_PLACEMENT_3D('',#5882,#4620,#4621);
#4017=AXIS2_PLACEMENT_3D('',#5886,#4623,#4624);
#4018=AXIS2_PLACEMENT_3D('',#5905,#4625,#4626);
#4019=AXIS2_PLACEMENT_3D('',#5923,#4627,#4628);
#4020=AXIS2_PLACEMENT_3D('',#5924,#4629,#4630);
#4021=AXIS2_PLACEMENT_3D('',#5926,#4631,#4632);
#4022=AXIS2_PLACEMENT_3D('',#5939,#4634,#4635);
#4023=AXIS2_PLACEMENT_3D('',#5958,#4636,#4637);
#4024=AXIS2_PLACEMENT_3D('',#5971,#4638,#4639);
#4025=AXIS2_PLACEMENT_3D('',#5973,#4640,#4641);
#4026=AXIS2_PLACEMENT_3D('',#5994,#4643,#4644);
#4027=AXIS2_PLACEMENT_3D('',#6013,#4645,#4646);
#4028=AXIS2_PLACEMENT_3D('',#6018,#4647,#4648);
#4029=AXIS2_PLACEMENT_3D('',#6020,#4649,#4650);
#4030=AXIS2_PLACEMENT_3D('',#6037,#4652,#4653);
#4031=AXIS2_PLACEMENT_3D('',#6056,#4654,#4655);
#4032=AXIS2_PLACEMENT_3D('',#6065,#4656,#4657);
#4033=AXIS2_PLACEMENT_3D('',#6067,#4658,#4659);
#4034=AXIS2_PLACEMENT_3D('',#6071,#4661,#4662);
#4035=AXIS2_PLACEMENT_3D('',#6090,#4663,#4664);
#4036=AXIS2_PLACEMENT_3D('',#6108,#4665,#4666);
#4037=AXIS2_PLACEMENT_3D('',#6109,#4667,#4668);
#4038=AXIS2_PLACEMENT_3D('',#6111,#4669,#4670);
#4039=AXIS2_PLACEMENT_3D('',#6115,#4672,#4673);
#4040=AXIS2_PLACEMENT_3D('',#6134,#4674,#4675);
#4041=AXIS2_PLACEMENT_3D('',#6152,#4676,#4677);
#4042=AXIS2_PLACEMENT_3D('',#6153,#4678,#4679);
#4043=AXIS2_PLACEMENT_3D('',#6155,#4680,#4681);
#4044=AXIS2_PLACEMENT_3D('',#6174,#4683,#4684);
#4045=AXIS2_PLACEMENT_3D('',#6193,#4685,#4686);
#4046=AXIS2_PLACEMENT_3D('',#6200,#4687,#4688);
#4047=AXIS2_PLACEMENT_3D('',#6202,#4689,#4690);
#4048=AXIS2_PLACEMENT_3D('',#6211,#4692,#4693);
#4049=AXIS2_PLACEMENT_3D('',#6230,#4694,#4695);
#4050=AXIS2_PLACEMENT_3D('',#6247,#4696,#4697);
#4051=AXIS2_PLACEMENT_3D('',#6248,#4698,#4699);
#4052=AXIS2_PLACEMENT_3D('',#6249,#4700,#4701);
#4053=AXIS2_PLACEMENT_3D('',#6250,#4702,#4703);
#4054=AXIS2_PLACEMENT_3D('',#6251,#4704,#4705);
#4055=AXIS2_PLACEMENT_3D('',#6252,#4706,#4707);
#4056=AXIS2_PLACEMENT_3D('',#6253,#4708,#4709);
#4057=AXIS2_PLACEMENT_3D('',#6254,#4710,#4711);
#4058=AXIS2_PLACEMENT_3D('',#6255,#4712,#4713);
#4059=AXIS2_PLACEMENT_3D('',#6256,#4714,#4715);
#4060=AXIS2_PLACEMENT_3D('',#6257,#4716,#4717);
#4061=AXIS2_PLACEMENT_3D('',#6259,#4718,#4719);
#4062=AXIS2_PLACEMENT_3D('',#6260,#4720,#4721);
#4063=AXIS2_PLACEMENT_3D('',#6261,#4722,#4723);
#4064=AXIS2_PLACEMENT_3D('',#6262,#4724,#4725);
#4065=AXIS2_PLACEMENT_3D('',#6263,#4726,#4727);
#4066=AXIS2_PLACEMENT_3D('',#6264,#4728,#4729);
#4067=AXIS2_PLACEMENT_3D('',#6265,#4730,#4731);
#4068=AXIS2_PLACEMENT_3D('',#6266,#4732,#4733);
#4069=AXIS2_PLACEMENT_3D('',#6267,#4734,#4735);
#4070=AXIS2_PLACEMENT_3D('',#6268,#4736,#4737);
#4071=AXIS2_PLACEMENT_3D('',#6269,#4738,#4739);
#4072=AXIS2_PLACEMENT_3D('',#6270,#4740,#4741);
#4073=AXIS2_PLACEMENT_3D('',#6271,#4742,#4743);
#4074=AXIS2_PLACEMENT_3D('',#6272,#4744,#4745);
#4075=AXIS2_PLACEMENT_3D('',#6273,#4746,#4747);
#4076=AXIS2_PLACEMENT_3D('',#6274,#4748,#4749);
#4077=AXIS2_PLACEMENT_3D('',#6275,#4750,#4751);
#4078=AXIS2_PLACEMENT_3D('',#6276,#4752,#4753);
#4079=AXIS2_PLACEMENT_3D('',#6277,#4754,#4755);
#4080=AXIS2_PLACEMENT_3D('',#6278,#4756,#4757);
#4081=AXIS2_PLACEMENT_3D('',#6279,#4758,#4759);
#4082=AXIS2_PLACEMENT_3D('',#6280,#4760,#4761);
#4083=AXIS2_PLACEMENT_3D('',#6282,#4762,#4763);
#4084=AXIS2_PLACEMENT_3D('',#6283,#4764,#4765);
#4085=AXIS2_PLACEMENT_3D('',#6285,#4766,#4767);
#4086=AXIS2_PLACEMENT_3D('',#6287,#4769,#4770);
#4087=AXIS2_PLACEMENT_3D('',#6289,#4771,#4772);
#4088=AXIS2_PLACEMENT_3D('',#6290,#4773,#4774);
#4089=AXIS2_PLACEMENT_3D('',#6292,#4776,#4777);
#4090=AXIS2_PLACEMENT_3D('',#6293,#4778,#4779);
#4091=AXIS2_PLACEMENT_3D('',#6313,#4780,#4781);
#4092=AXIS2_PLACEMENT_3D('',#6325,#4783,#4784);
#4093=AXIS2_PLACEMENT_3D('',#6339,#4785,#4786);
#4094=AXIS2_PLACEMENT_3D('',#6340,#4787,#4788);
#4095=AXIS2_PLACEMENT_3D('',#6360,#4789,#4790);
#4096=AXIS2_PLACEMENT_3D('',#6379,#4791,#4792);
#4097=AXIS2_PLACEMENT_3D('',#6382,#4794,#4795);
#4098=AXIS2_PLACEMENT_3D('',#6383,#4796,#4797);
#4099=AXIS2_PLACEMENT_3D('',#6384,#4798,#4799);
#4100=AXIS2_PLACEMENT_3D('',#6404,#4800,#4801);
#4101=AXIS2_PLACEMENT_3D('',#6407,#4803,#4804);
#4102=AXIS2_PLACEMENT_3D('',#6409,#4805,#4806);
#4103=AXIS2_PLACEMENT_3D('',#6427,#4807,#4808);
#4104=AXIS2_PLACEMENT_3D('',#6428,#4809,#4810);
#4105=AXIS2_PLACEMENT_3D('',#6446,#4811,#4812);
#4106=AXIS2_PLACEMENT_3D('',#6465,#4813,#4814);
#4107=AXIS2_PLACEMENT_3D('',#6474,#4816,#4817);
#4108=AXIS2_PLACEMENT_3D('',#6475,#4818,#4819);
#4109=AXIS2_PLACEMENT_3D('',#6483,#4820,#4821);
#4110=AXIS2_PLACEMENT_3D('',#6502,#4822,#4823);
#4111=AXIS2_PLACEMENT_3D('',#6521,#4825,#4826);
#4112=AXIS2_PLACEMENT_3D('',#6522,#4827,#4828);
#4113=AXIS2_PLACEMENT_3D('',#6536,#4829,#4830);
#4114=AXIS2_PLACEMENT_3D('',#6555,#4831,#4832);
#4115=AXIS2_PLACEMENT_3D('',#6568,#4834,#4835);
#4116=AXIS2_PLACEMENT_3D('',#6569,#4836,#4837);
#4117=AXIS2_PLACEMENT_3D('',#6589,#4838,#4839);
#4118=AXIS2_PLACEMENT_3D('',#6608,#4840,#4841);
#4119=AXIS2_PLACEMENT_3D('',#6611,#4843,#4844);
#4120=AXIS2_PLACEMENT_3D('',#6612,#4845,#4846);
#4121=AXIS2_PLACEMENT_3D('',#6613,#4847,#4848);
#4122=AXIS2_PLACEMENT_3D('',#6633,#4849,#4850);
#4123=AXIS2_PLACEMENT_3D('',#6652,#4851,#4852);
#4124=AXIS2_PLACEMENT_3D('',#6655,#4854,#4855);
#4125=AXIS2_PLACEMENT_3D('',#6656,#4856,#4857);
#4126=AXIS2_PLACEMENT_3D('',#6657,#4858,#4859);
#4127=AXIS2_PLACEMENT_3D('',#6677,#4860,#4861);
#4128=AXIS2_PLACEMENT_3D('',#6693,#4863,#4864);
#4129=AXIS2_PLACEMENT_3D('',#6703,#4865,#4866);
#4130=AXIS2_PLACEMENT_3D('',#6704,#4867,#4868);
#4131=AXIS2_PLACEMENT_3D('',#6724,#4869,#4870);
#4132=AXIS2_PLACEMENT_3D('',#6732,#4872,#4873);
#4133=AXIS2_PLACEMENT_3D('',#6750,#4874,#4875);
#4134=AXIS2_PLACEMENT_3D('',#6751,#4876,#4877);
#4135=AXIS2_PLACEMENT_3D('',#6752,#4878,#4879);
#4136=AXIS2_PLACEMENT_3D('',#6753,#4880,#4881);
#4137=AXIS2_PLACEMENT_3D('',#6754,#4882,#4883);
#4138=AXIS2_PLACEMENT_3D('',#6755,#4884,#4885);
#4139=AXIS2_PLACEMENT_3D('',#6756,#4886,#4887);
#4140=AXIS2_PLACEMENT_3D('',#6757,#4888,#4889);
#4141=AXIS2_PLACEMENT_3D('',#6758,#4890,#4891);
#4142=AXIS2_PLACEMENT_3D('',#6759,#4892,#4893);
#4143=AXIS2_PLACEMENT_3D('',#6760,#4894,#4895);
#4144=AXIS2_PLACEMENT_3D('',#6761,#4896,#4897);
#4145=AXIS2_PLACEMENT_3D('',#6763,#4898,#4899);
#4146=AXIS2_PLACEMENT_3D('',#6764,#4900,#4901);
#4147=AXIS2_PLACEMENT_3D('',#6765,#4902,#4903);
#4148=AXIS2_PLACEMENT_3D('',#6766,#4904,#4905);
#4149=AXIS2_PLACEMENT_3D('',#6767,#4906,#4907);
#4150=AXIS2_PLACEMENT_3D('',#6768,#4908,#4909);
#4151=AXIS2_PLACEMENT_3D('',#6769,#4910,#4911);
#4152=AXIS2_PLACEMENT_3D('',#6770,#4912,#4913);
#4153=AXIS2_PLACEMENT_3D('',#6771,#4914,#4915);
#4154=AXIS2_PLACEMENT_3D('',#6772,#4916,#4917);
#4155=AXIS2_PLACEMENT_3D('',#6773,#4918,#4919);
#4156=AXIS2_PLACEMENT_3D('',#6774,#4920,#4921);
#4157=AXIS2_PLACEMENT_3D('',#6775,#4922,#4923);
#4158=AXIS2_PLACEMENT_3D('',#6776,#4924,#4925);
#4159=AXIS2_PLACEMENT_3D('',#6777,#4926,#4927);
#4160=AXIS2_PLACEMENT_3D('',#6778,#4928,#4929);
#4161=AXIS2_PLACEMENT_3D('',#6779,#4930,#4931);
#4162=AXIS2_PLACEMENT_3D('',#6780,#4932,#4933);
#4163=AXIS2_PLACEMENT_3D('',#6781,#4934,#4935);
#4164=AXIS2_PLACEMENT_3D('',#6782,#4936,#4937);
#4165=AXIS2_PLACEMENT_3D('',#6783,#4938,#4939);
#4166=AXIS2_PLACEMENT_3D('',#6784,#4940,#4941);
#4167=AXIS2_PLACEMENT_3D('',#6786,#4942,#4943);
#4168=AXIS2_PLACEMENT_3D('',#6788,#4944,#4945);
#4169=AXIS2_PLACEMENT_3D('',#6789,#4946,#4947);
#4170=AXIS2_PLACEMENT_3D('',#6791,#4948,#4949);
#4171=AXIS2_PLACEMENT_3D('',#6793,#4951,#4952);
#4172=AXIS2_PLACEMENT_3D('',#6794,#4953,#4954);
#4173=AXIS2_PLACEMENT_3D('',#6796,#4956,#4957);
#4174=AXIS2_PLACEMENT_3D('',#6797,#4958,#4959);
#4175=AXIS2_PLACEMENT_3D('',#6800,#4960,#4961);
#4176=AXIS2_PLACEMENT_3D('',#6801,#4962,#4963);
#4177=AXIS2_PLACEMENT_3D('',#6804,#4964,#4965);
#4178=AXIS2_PLACEMENT_3D('',#6805,#4966,#4967);
#4179=AXIS2_PLACEMENT_3D('',#6808,#4968,#4969);
#4180=AXIS2_PLACEMENT_3D('',#6809,#4970,#4971);
#4181=AXIS2_PLACEMENT_3D('',#6812,#4972,#4973);
#4182=AXIS2_PLACEMENT_3D('',#6813,#4974,#4975);
#4183=AXIS2_PLACEMENT_3D('',#6816,#4976,#4977);
#4184=AXIS2_PLACEMENT_3D('',#6817,#4978,#4979);
#4185=AXIS2_PLACEMENT_3D('',#6820,#4980,#4981);
#4186=AXIS2_PLACEMENT_3D('',#6821,#4982,#4983);
#4187=AXIS2_PLACEMENT_3D('',#6824,#4984,#4985);
#4188=AXIS2_PLACEMENT_3D('',#6825,#4986,#4987);
#4189=AXIS2_PLACEMENT_3D('',#6828,#4988,#4989);
#4190=AXIS2_PLACEMENT_3D('',#6829,#4990,#4991);
#4191=AXIS2_PLACEMENT_3D('',#6832,#4992,#4993);
#4192=AXIS2_PLACEMENT_3D('',#6833,#4994,#4995);
#4193=AXIS2_PLACEMENT_3D('',#6836,#4996,#4997);
#4194=AXIS2_PLACEMENT_3D('',#6837,#4998,#4999);
#4195=AXIS2_PLACEMENT_3D('',#6838,#5000,#5001);
#4196=AXIS2_PLACEMENT_3D('',#6839,#5002,#5003);
#4197=AXIS2_PLACEMENT_3D('',#6840,#5004,#5005);
#4198=AXIS2_PLACEMENT_3D('',#6841,#5006,#5007);
#4199=AXIS2_PLACEMENT_3D('',#6843,#5008,#5009);
#4200=AXIS2_PLACEMENT_3D('',#6846,#5011,#5012);
#4201=AXIS2_PLACEMENT_3D('',#6847,#5013,#5014);
#4202=AXIS2_PLACEMENT_3D('',#6849,#5015,#5016);
#4203=AXIS2_PLACEMENT_3D('',#6852,#5018,#5019);
#4204=AXIS2_PLACEMENT_3D('',#6853,#5020,#5021);
#4205=AXIS2_PLACEMENT_3D('',#6854,#5022,#5023);
#4206=AXIS2_PLACEMENT_3D('',#6855,#5024,#5025);
#4207=AXIS2_PLACEMENT_3D('',#6856,#5026,#5027);
#4208=AXIS2_PLACEMENT_3D('',#6868,#5029,#5030);
#4209=AXIS2_PLACEMENT_3D('',#6884,#5031,#5032);
#4210=AXIS2_PLACEMENT_3D('',#6886,#5033,#5034);
#4211=AXIS2_PLACEMENT_3D('',#6912,#5036,#5037);
#4212=AXIS2_PLACEMENT_3D('',#6915,#5040,#5041);
#4213=AXIS2_PLACEMENT_3D('',#6917,#5043,#5044);
#4214=AXIS2_PLACEMENT_3D('',#6919,#5046,#5047);
#4215=AXIS2_PLACEMENT_3D('',#6921,#5048,#5049);
#4216=AXIS2_PLACEMENT_3D('',#6924,#5051,#5052);
#4217=AXIS2_PLACEMENT_3D('',#6925,#5053,#5054);
#4218=AXIS2_PLACEMENT_3D('',#6927,#5056,#5057);
#4219=AXIS2_PLACEMENT_3D('',#6929,#5059,#5060);
#4220=AXIS2_PLACEMENT_3D('',#6930,#5061,#5062);
#4221=AXIS2_PLACEMENT_3D('',#6931,#5063,#5064);
#4222=AXIS2_PLACEMENT_3D('',#6932,#5065,#5066);
#4223=AXIS2_PLACEMENT_3D('',#6933,#5067,#5068);
#4224=AXIS2_PLACEMENT_3D('',#6934,#5069,#5070);
#4225=AXIS2_PLACEMENT_3D('',#6935,#5071,#5072);
#4226=AXIS2_PLACEMENT_3D('',#6936,#5073,#5074);
#4227=AXIS2_PLACEMENT_3D('',#6937,#5075,#5076);
#4228=AXIS2_PLACEMENT_3D('',#6938,#5077,#5078);
#4229=AXIS2_PLACEMENT_3D('',#6939,#5079,#5080);
#4230=AXIS2_PLACEMENT_3D('',#6941,#5081,#5082);
#4231=AXIS2_PLACEMENT_3D('',#6944,#5084,#5085);
#4232=AXIS2_PLACEMENT_3D('',#6945,#5086,#5087);
#4233=AXIS2_PLACEMENT_3D('',#6948,#5088,#5089);
#4234=AXIS2_PLACEMENT_3D('',#6952,#5091,#5092);
#4235=AXIS2_PLACEMENT_3D('',#6954,#5094,#5095);
#4236=AXIS2_PLACEMENT_3D('',#6959,#5097,#5098);
#4237=AXIS2_PLACEMENT_3D('',#6962,#5100,#5101);
#4238=AXIS2_PLACEMENT_3D('',#6963,#5102,#5103);
#4239=AXIS2_PLACEMENT_3D('',#6981,#5113,#5114);
#4240=AXIS2_PLACEMENT_3D('',#6985,#5117,#5118);
#4241=AXIS2_PLACEMENT_3D('',#6989,#5121,#5122);
#4242=AXIS2_PLACEMENT_3D('',#7007,#5132,#5133);
#4243=AXIS2_PLACEMENT_3D('',#7011,#5136,#5137);
#4244=AXIS2_PLACEMENT_3D('',#7015,#5140,#5141);
#4245=AXIS2_PLACEMENT_3D('',#7019,#5144,#5145);
#4246=AXIS2_PLACEMENT_3D('',#7021,#5147,#5148);
#4247=AXIS2_PLACEMENT_3D('',#7029,#5154,#5155);
#4248=AXIS2_PLACEMENT_3D('',#7034,#5159,#5160);
#4249=AXIS2_PLACEMENT_3D('',#7035,#5161,#5162);
#4250=AXIS2_PLACEMENT_3D('',#7037,#5164,#5165);
#4251=AXIS2_PLACEMENT_3D('',#7038,#5166,#5167);
#4252=AXIS2_PLACEMENT_3D('',#7040,#5169,#5170);
#4253=AXIS2_PLACEMENT_3D('',#7042,#5172,#5173);
#4254=AXIS2_PLACEMENT_3D('',#7043,#5174,#5175);
#4255=AXIS2_PLACEMENT_3D('',#7044,#5176,#5177);
#4256=AXIS2_PLACEMENT_3D('',#7046,#5178,#5179);
#4257=AXIS2_PLACEMENT_3D('',#7049,#5181,#5182);
#4258=AXIS2_PLACEMENT_3D('',#7050,#5183,#5184);
#4259=AXIS2_PLACEMENT_3D('',#7052,#5185,#5186);
#4260=AXIS2_PLACEMENT_3D('',#7055,#5188,#5189);
#4261=AXIS2_PLACEMENT_3D('',#7056,#5190,#5191);
#4262=AXIS2_PLACEMENT_3D('',#7057,#5192,#5193);
#4263=AXIS2_PLACEMENT_3D('',#7058,#5194,#5195);
#4264=AXIS2_PLACEMENT_3D('',#7059,#5196,#5197);
#4265=AXIS2_PLACEMENT_3D('',#7061,#5198,#5199);
#4266=AXIS2_PLACEMENT_3D('',#7064,#5201,#5202);
#4267=AXIS2_PLACEMENT_3D('',#7065,#5203,#5204);
#4268=AXIS2_PLACEMENT_3D('',#7066,#5205,#5206);
#4269=AXIS2_PLACEMENT_3D('',#7068,#5207,#5208);
#4270=AXIS2_PLACEMENT_3D('',#7070,#5209,#5210);
#4271=AXIS2_PLACEMENT_3D('',#7071,#5211,#5212);
#4272=AXIS2_PLACEMENT_3D('',#7074,#5214,#5215);
#4273=AXIS2_PLACEMENT_3D('',#7075,#5216,#5217);
#4274=AXIS2_PLACEMENT_3D('',#7076,#5218,#5219);
#4275=AXIS2_PLACEMENT_3D('',#7078,#5220,#5221);
#4276=AXIS2_PLACEMENT_3D('',#7080,#5223,#5224);
#4277=AXIS2_PLACEMENT_3D('',#7081,#5225,#5226);
#4278=AXIS2_PLACEMENT_3D('',#7082,#5227,#5228);
#4279=AXIS2_PLACEMENT_3D('',#7084,#5229,#5230);
#4280=AXIS2_PLACEMENT_3D('',#7087,#5232,#5233);
#4281=AXIS2_PLACEMENT_3D('',#7088,#5234,#5235);
#4282=AXIS2_PLACEMENT_3D('',#7090,#5236,#5237);
#4283=AXIS2_PLACEMENT_3D('',#7093,#5239,#5240);
#4284=AXIS2_PLACEMENT_3D('',#7094,#5241,#5242);
#4285=AXIS2_PLACEMENT_3D('',#7095,#5243,#5244);
#4286=AXIS2_PLACEMENT_3D('',#7096,#5245,#5246);
#4287=AXIS2_PLACEMENT_3D('',#7097,#5247,#5248);
#4288=AXIS2_PLACEMENT_3D('',#7099,#5249,#5250);
#4289=AXIS2_PLACEMENT_3D('',#7102,#5252,#5253);
#4290=AXIS2_PLACEMENT_3D('',#7103,#5254,#5255);
#4291=AXIS2_PLACEMENT_3D('',#7105,#5256,#5257);
#4292=AXIS2_PLACEMENT_3D('',#7108,#5259,#5260);
#4293=AXIS2_PLACEMENT_3D('',#7109,#5261,#5262);
#4294=AXIS2_PLACEMENT_3D('',#7110,#5263,#5264);
#4295=AXIS2_PLACEMENT_3D('',#7111,#5265,#5266);
#4296=AXIS2_PLACEMENT_3D('',#7112,#5267,#5268);
#4297=AXIS2_PLACEMENT_3D('',#7121,#5273,#5274);
#4298=AXIS2_PLACEMENT_3D('',#7127,#5278,#5279);
#4299=AXIS2_PLACEMENT_3D('',#7133,#5283,#5284);
#4300=AXIS2_PLACEMENT_3D('',#7139,#5288,#5289);
#4301=AXIS2_PLACEMENT_3D('',#7145,#5293,#5294);
#4302=AXIS2_PLACEMENT_3D('',#7148,#5297,#5298);
#4303=AXIS2_PLACEMENT_3D('',#7149,#5299,#5300);
#4304=AXIS2_PLACEMENT_3D('',#7150,#5301,#5302);
#4305=AXIS2_PLACEMENT_3D('',#7152,#5303,#5304);
#4306=AXIS2_PLACEMENT_3D('',#7153,#5305,#5306);
#4307=AXIS2_PLACEMENT_3D('',#7155,#5307,#5308);
#4308=AXIS2_PLACEMENT_3D('',#7156,#5309,#5310);
#4309=AXIS2_PLACEMENT_3D('',#7158,#5311,#5312);
#4310=AXIS2_PLACEMENT_3D('',#7160,#5314,#5315);
#4311=AXIS2_PLACEMENT_3D('',#7162,#5316,#5317);
#4312=AXIS2_PLACEMENT_3D('',#7164,#5319,#5320);
#4313=AXIS2_PLACEMENT_3D('',#7166,#5321,#5322);
#4314=AXIS2_PLACEMENT_3D('',#7168,#5324,#5325);
#4315=AXIS2_PLACEMENT_3D('',#7170,#5326,#5327);
#4316=AXIS2_PLACEMENT_3D('',#7171,#5328,#5329);
#4317=AXIS2_PLACEMENT_3D('',#7173,#5330,#5331);
#4318=AXIS2_PLACEMENT_3D('',#7175,#5333,#5334);
#4319=AXIS2_PLACEMENT_3D('',#7177,#5336,#5337);
#4320=AXIS2_PLACEMENT_3D('',#7178,#5338,#5339);
#4321=AXIS2_PLACEMENT_3D('',#7179,#5340,#5341);
#4322=AXIS2_PLACEMENT_3D('',#7180,#5342,#5343);
#4323=AXIS2_PLACEMENT_3D('',#7181,#5344,#5345);
#4324=AXIS2_PLACEMENT_3D('',#7182,#5346,#5347);
#4325=AXIS2_PLACEMENT_3D('',#7183,#5348,#5349);
#4326=AXIS2_PLACEMENT_3D('',#7184,#5350,#5351);
#4327=AXIS2_PLACEMENT_3D('',#7185,#5352,#5353);
#4328=AXIS2_PLACEMENT_3D('',#7186,#5354,#5355);
#4329=AXIS2_PLACEMENT_3D('',#7188,#5356,#5357);
#4330=AXIS2_PLACEMENT_3D('',#7191,#5359,#5360);
#4331=AXIS2_PLACEMENT_3D('',#7192,#5361,#5362);
#4332=AXIS2_PLACEMENT_3D('',#7194,#5363,#5364);
#4333=AXIS2_PLACEMENT_3D('',#7195,#5365,#5366);
#4334=AXIS2_PLACEMENT_3D('',#7197,#5367,#5368);
#4335=AXIS2_PLACEMENT_3D('',#7200,#5370,#5371);
#4336=AXIS2_PLACEMENT_3D('',#7201,#5372,#5373);
#4337=AXIS2_PLACEMENT_3D('',#7203,#5374,#5375);
#4338=AXIS2_PLACEMENT_3D('',#7204,#5376,#5377);
#4339=AXIS2_PLACEMENT_3D('',#7206,#5379,#5380);
#4340=AXIS2_PLACEMENT_3D('',#7208,#5381,#5382);
#4341=AXIS2_PLACEMENT_3D('',#7211,#5384,#5385);
#4342=AXIS2_PLACEMENT_3D('',#7212,#5386,#5387);
#4343=AXIS2_PLACEMENT_3D('',#7213,#5388,#5389);
#4344=AXIS2_PLACEMENT_3D('',#7214,#5390,#5391);
#4345=AXIS2_PLACEMENT_3D('',#7215,#5392,#5393);
#4346=AXIS2_PLACEMENT_3D('',#7216,#5394,#5395);
#4347=AXIS2_PLACEMENT_3D('',#7219,#5396,#5397);
#4348=AXIS2_PLACEMENT_3D('',#7220,#5398,#5399);
#4349=AXIS2_PLACEMENT_3D('',#7222,#5400,#5401);
#4350=AXIS2_PLACEMENT_3D('',#7224,#5402,#5403);
#4351=AXIS2_PLACEMENT_3D('',#7225,#5404,#5405);
#4352=AXIS2_PLACEMENT_3D('',#7226,#5406,#5407);
#4353=AXIS2_PLACEMENT_3D('',#7229,#5409,#5410);
#4354=AXIS2_PLACEMENT_3D('',#7230,#5411,#5412);
#4355=AXIS2_PLACEMENT_3D('',#7232,#5413,#5414);
#4356=AXIS2_PLACEMENT_3D('',#7235,#5416,#5417);
#4357=AXIS2_PLACEMENT_3D('',#7236,#5418,#5419);
#4358=AXIS2_PLACEMENT_3D('',#7239,#5421,#5422);
#4359=AXIS2_PLACEMENT_3D('',#7240,#5423,#5424);
#4360=AXIS2_PLACEMENT_3D('',#7241,#5425,#5426);
#4361=AXIS2_PLACEMENT_3D('',#7243,#5427,#5428);
#4362=AXIS2_PLACEMENT_3D('',#7245,#5430,#5431);
#4363=AXIS2_PLACEMENT_3D('',#7247,#5432,#5433);
#4364=AXIS2_PLACEMENT_3D('',#7248,#5434,#5435);
#4365=AXIS2_PLACEMENT_3D('',#7250,#5437,#5438);
#4366=AXIS2_PLACEMENT_3D('',#7251,#5439,#5440);
#4367=AXIS2_PLACEMENT_3D('',#7254,#5441,#5442);
#4368=AXIS2_PLACEMENT_3D('',#7255,#5443,#5444);
#4369=AXIS2_PLACEMENT_3D('',#7257,#5445,#5446);
#4370=AXIS2_PLACEMENT_3D('',#7259,#5447,#5448);
#4371=AXIS2_PLACEMENT_3D('',#7260,#5449,#5450);
#4372=AXIS2_PLACEMENT_3D('',#7261,#5451,#5452);
#4373=AXIS2_PLACEMENT_3D('',#7263,#5453,#5454);
#4374=AXIS2_PLACEMENT_3D('',#7265,#5456,#5457);
#4375=AXIS2_PLACEMENT_3D('',#7267,#5458,#5459);
#4376=AXIS2_PLACEMENT_3D('',#7269,#5460,#5461);
#4377=AXIS2_PLACEMENT_3D('',#7270,#5462,#5463);
#4378=AXIS2_PLACEMENT_3D('',#7272,#5464,#5465);
#4379=AXIS2_PLACEMENT_3D('',#7274,#5467,#5468);
#4380=AXIS2_PLACEMENT_3D('',#7276,#5469,#5470);
#4381=AXIS2_PLACEMENT_3D('',#7278,#5472,#5473);
#4382=AXIS2_PLACEMENT_3D('',#7280,#5474,#5475);
#4383=AXIS2_PLACEMENT_3D('',#7282,#5477,#5478);
#4384=AXIS2_PLACEMENT_3D('',#7283,#5479,#5480);
#4385=AXIS2_PLACEMENT_3D('',#7285,#5482,#5483);
#4386=AXIS2_PLACEMENT_3D('',#7286,#5484,#5485);
#4387=AXIS2_PLACEMENT_3D('',#7289,#5486,#5487);
#4388=AXIS2_PLACEMENT_3D('',#7290,#5488,#5489);
#4389=AXIS2_PLACEMENT_3D('',#7293,#5490,#5491);
#4390=AXIS2_PLACEMENT_3D('',#7294,#5492,#5493);
#4391=AXIS2_PLACEMENT_3D('',#7297,#5494,#5495);
#4392=AXIS2_PLACEMENT_3D('',#7298,#5496,#5497);
#4393=AXIS2_PLACEMENT_3D('',#7301,#5498,#5499);
#4394=AXIS2_PLACEMENT_3D('',#7302,#5500,#5501);
#4395=AXIS2_PLACEMENT_3D('',#7305,#5502,#5503);
#4396=AXIS2_PLACEMENT_3D('',#7306,#5504,#5505);
#4397=AXIS2_PLACEMENT_3D('',#7309,#5506,#5507);
#4398=AXIS2_PLACEMENT_3D('',#7310,#5508,#5509);
#4399=AXIS2_PLACEMENT_3D('',#7313,#5510,#5511);
#4400=AXIS2_PLACEMENT_3D('',#7314,#5512,#5513);
#4401=AXIS2_PLACEMENT_3D('',#7315,#5514,#5515);
#4402=AXIS2_PLACEMENT_3D('',#7341,#5516,#5517);
#4403=AXIS2_PLACEMENT_3D('',#7365,#5518,#5519);
#4404=AXIS2_PLACEMENT_3D('',#7366,#5520,#5521);
#4405=AXIS2_PLACEMENT_3D('',#7368,#5522,#5523);
#4406=AXIS2_PLACEMENT_3D('',#7393,#5524,#5525);
#4407=AXIS2_PLACEMENT_3D('',#7418,#5526,#5527);
#4408=AXIS2_PLACEMENT_3D('',#7421,#5529,#5530);
#4409=AXIS2_PLACEMENT_3D('',#7423,#5531,#5532);
#4410=AXIS2_PLACEMENT_3D('',#7448,#5533,#5534);
#4411=AXIS2_PLACEMENT_3D('',#7473,#5535,#5536);
#4412=AXIS2_PLACEMENT_3D('',#7498,#5537,#5538);
#4413=AXIS2_PLACEMENT_3D('',#7522,#5539,#5540);
#4414=AXIS2_PLACEMENT_3D('',#7523,#5541,#5542);
#4415=AXIS2_PLACEMENT_3D('',#7525,#5543,#5544);
#4416=AXIS2_PLACEMENT_3D('',#7526,#5545,#5546);
#4417=AXIS2_PLACEMENT_3D('',#7527,#5547,#5548);
#4418=AXIS2_PLACEMENT_3D('',#7551,#5549,#5550);
#4419=AXIS2_PLACEMENT_3D('',#7552,#5551,#5552);
#4420=AXIS2_PLACEMENT_3D('',#7554,#5553,#5554);
#4421=AXIS2_PLACEMENT_3D('',#7555,#5555,#5556);
#4422=AXIS2_PLACEMENT_3D('',#7556,#5557,#5558);
#4423=AXIS2_PLACEMENT_3D('',#7580,#5559,#5560);
#4424=AXIS2_PLACEMENT_3D('',#7581,#5561,#5562);
#4425=AXIS2_PLACEMENT_3D('',#7583,#5563,#5564);
#4426=AXIS2_PLACEMENT_3D('',#7585,#5565,#5566);
#4427=AXIS2_PLACEMENT_3D('',#7586,#5567,#5568);
#4428=AXIS2_PLACEMENT_3D('',#7587,#5569,#5570);
#4429=AXIS2_PLACEMENT_3D('',#7611,#5571,#5572);
#4430=AXIS2_PLACEMENT_3D('',#7612,#5573,#5574);
#4431=AXIS2_PLACEMENT_3D('',#7614,#5575,#5576);
#4432=AXIS2_PLACEMENT_3D('',#7615,#5577,#5578);
#4433=AXIS2_PLACEMENT_3D('',#7616,#5579,#5580);
#4434=AXIS2_PLACEMENT_3D('',#7640,#5581,#5582);
#4435=AXIS2_PLACEMENT_3D('',#7641,#5583,#5584);
#4436=AXIS2_PLACEMENT_3D('',#7643,#5585,#5586);
#4437=AXIS2_PLACEMENT_3D('',#7644,#5587,#5588);
#4438=AXIS2_PLACEMENT_3D('',#7645,#5589,#5590);
#4439=AXIS2_PLACEMENT_3D('',#7669,#5591,#5592);
#4440=AXIS2_PLACEMENT_3D('',#7670,#5593,#5594);
#4441=AXIS2_PLACEMENT_3D('',#7672,#5595,#5596);
#4442=AXIS2_PLACEMENT_3D('',#7675,#5598,#5599);
#4443=AXIS2_PLACEMENT_3D('',#7699,#5600,#5601);
#4444=AXIS2_PLACEMENT_3D('',#7700,#5602,#5603);
#4445=AXIS2_PLACEMENT_3D('',#7701,#5604,#5605);
#4446=AXIS2_PLACEMENT_3D('',#7702,#5606,#5607);
#4447=AXIS2_PLACEMENT_3D('',#7703,#5608,#5609);
#4448=AXIS2_PLACEMENT_3D('',#7704,#5610,#5611);
#4449=AXIS2_PLACEMENT_3D('',#7705,#5612,#5613);
#4450=AXIS2_PLACEMENT_3D('',#7706,#5614,#5615);
#4451=AXIS2_PLACEMENT_3D('',#7707,#5616,#5617);
#4452=AXIS2_PLACEMENT_3D('',#7709,#5618,#5619);
#4453=AXIS2_PLACEMENT_3D('',#7711,#5620,#5621);
#4454=AXIS2_PLACEMENT_3D('',#7712,#5622,#5623);
#4455=AXIS2_PLACEMENT_3D('',#7714,#5624,#5625);
#4456=AXIS2_PLACEMENT_3D('',#7716,#5627,#5628);
#4457=AXIS2_PLACEMENT_3D('',#7718,#5629,#5630);
#4458=AXIS2_PLACEMENT_3D('',#7719,#5631,#5632);
#4459=AXIS2_PLACEMENT_3D('',#7721,#5634,#5635);
#4460=AXIS2_PLACEMENT_3D('',#7723,#5636,#5637);
#4461=AXIS2_PLACEMENT_3D('',#7725,#5638,#5639);
#4462=AXIS2_PLACEMENT_3D('',#7726,#5640,#5641);
#4463=AXIS2_PLACEMENT_3D('',#7728,#5642,#5643);
#4464=AXIS2_PLACEMENT_3D('',#7730,#5645,#5646);
#4465=AXIS2_PLACEMENT_3D('',#7732,#5647,#5648);
#4466=AXIS2_PLACEMENT_3D('',#7733,#5649,#5650);
#4467=AXIS2_PLACEMENT_3D('',#7735,#5652,#5653);
#4468=AXIS2_PLACEMENT_3D('',#7736,#5654,#5655);
#4469=AXIS2_PLACEMENT_3D('',#7737,#5656,#5657);
#4470=AXIS2_PLACEMENT_3D('',#7738,#5658,#5659);
#4471=AXIS2_PLACEMENT_3D('',#7739,#5660,#5661);
#4472=AXIS2_PLACEMENT_3D('',#7740,#5662,#5663);
#4473=AXIS2_PLACEMENT_3D('',#7741,#5664,#5665);
#4474=AXIS2_PLACEMENT_3D('',#7743,#5666,#5667);
#4475=AXIS2_PLACEMENT_3D('',#7746,#5669,#5670);
#4476=AXIS2_PLACEMENT_3D('',#7747,#5671,#5672);
#4477=AXIS2_PLACEMENT_3D('',#7749,#5673,#5674);
#4478=AXIS2_PLACEMENT_3D('',#7752,#5676,#5677);
#4479=AXIS2_PLACEMENT_3D('',#7753,#5678,#5679);
#4480=AXIS2_PLACEMENT_3D('',#7754,#5680,#5681);
#4481=AXIS2_PLACEMENT_3D('',#7755,#5682,#5683);
#4482=AXIS2_PLACEMENT_3D('',#7756,#5684,#5685);
#4483=AXIS2_PLACEMENT_3D('',#7757,#5686,#5687);
#4484=AXIS2_PLACEMENT_3D('',#7758,#5688,#5689);
#4485=AXIS2_PLACEMENT_3D('',#7759,#5690,#5691);
#4486=AXIS2_PLACEMENT_3D('',#7760,#5692,#5693);
#4487=AXIS2_PLACEMENT_3D('',#7761,#5694,#5695);
#4488=AXIS2_PLACEMENT_3D('',#7762,#5696,#5697);
#4489=DIRECTION('axis',(0.,0.,1.));
#4490=DIRECTION('refdir',(1.,0.,0.));
#4491=DIRECTION('axis',(0.,0.,1.));
#4492=DIRECTION('refdir',(1.,0.,0.));
#4493=DIRECTION('axis',(0.,0.,1.));
#4494=DIRECTION('refdir',(1.,0.,0.));
#4495=DIRECTION('center_axis',(0.,0.,1.));
#4496=DIRECTION('ref_axis',(1.,0.,0.));
#4497=DIRECTION('center_axis',(0.,0.,1.));
#4498=DIRECTION('ref_axis',(1.,0.,0.));
#4499=DIRECTION('',(0.,0.,1.));
#4500=DIRECTION('center_axis',(0.,0.,-1.));
#4501=DIRECTION('ref_axis',(1.,0.,0.));
#4502=DIRECTION('center_axis',(0.,0.,1.));
#4503=DIRECTION('ref_axis',(1.,0.,0.));
#4504=DIRECTION('center_axis',(0.,0.,1.));
#4505=DIRECTION('ref_axis',(1.,0.,0.));
#4506=DIRECTION('',(0.,0.,1.));
#4507=DIRECTION('center_axis',(0.,0.,-1.));
#4508=DIRECTION('ref_axis',(1.,0.,0.));
#4509=DIRECTION('center_axis',(0.,0.,1.));
#4510=DIRECTION('ref_axis',(1.,0.,0.));
#4511=DIRECTION('center_axis',(0.,0.,1.));
#4512=DIRECTION('ref_axis',(1.,0.,0.));
#4513=DIRECTION('',(0.,0.,1.));
#4514=DIRECTION('center_axis',(0.,0.,-1.));
#4515=DIRECTION('ref_axis',(1.,0.,0.));
#4516=DIRECTION('center_axis',(0.,0.,1.));
#4517=DIRECTION('ref_axis',(1.,0.,0.));
#4518=DIRECTION('center_axis',(0.,0.,1.));
#4519=DIRECTION('ref_axis',(1.,0.,0.));
#4520=DIRECTION('',(0.,0.,1.));
#4521=DIRECTION('center_axis',(0.,0.,-1.));
#4522=DIRECTION('ref_axis',(1.,0.,0.));
#4523=DIRECTION('center_axis',(0.,0.,1.));
#4524=DIRECTION('ref_axis',(1.,0.,0.));
#4525=DIRECTION('center_axis',(0.,0.,1.));
#4526=DIRECTION('ref_axis',(1.,0.,0.));
#4527=DIRECTION('',(0.,0.,1.));
#4528=DIRECTION('center_axis',(0.,0.,-1.));
#4529=DIRECTION('ref_axis',(1.,0.,0.));
#4530=DIRECTION('center_axis',(0.,1.,0.));
#4531=DIRECTION('ref_axis',(-1.,0.,0.));
#4532=DIRECTION('',(-1.,0.,0.));
#4533=DIRECTION('',(0.,0.,1.));
#4534=DIRECTION('',(-1.,0.,0.));
#4535=DIRECTION('',(0.,0.,1.));
#4536=DIRECTION('center_axis',(1.,0.,0.));
#4537=DIRECTION('ref_axis',(0.,1.,0.));
#4538=DIRECTION('',(0.,1.,0.));
#4539=DIRECTION('',(0.,1.,0.));
#4540=DIRECTION('',(0.,0.,1.));
#4541=DIRECTION('center_axis',(0.,-1.,0.));
#4542=DIRECTION('ref_axis',(1.,0.,0.));
#4543=DIRECTION('',(1.,0.,0.));
#4544=DIRECTION('',(1.,0.,0.));
#4545=DIRECTION('',(0.,0.,1.));
#4546=DIRECTION('center_axis',(-1.,0.,0.));
#4547=DIRECTION('ref_axis',(0.,-1.,0.));
#4548=DIRECTION('',(0.,-1.,0.));
#4549=DIRECTION('',(0.,-1.,0.));
#4550=DIRECTION('center_axis',(0.,0.,1.));
#4551=DIRECTION('ref_axis',(1.,0.,0.));
#4552=DIRECTION('center_axis',(0.,0.,1.));
#4553=DIRECTION('ref_axis',(1.,0.,0.));
#4554=DIRECTION('axis',(0.,0.,1.));
#4555=DIRECTION('refdir',(1.,0.,0.));
#4556=DIRECTION('center_axis',(0.,0.,1.));
#4557=DIRECTION('ref_axis',(1.,0.,0.));
#4558=DIRECTION('center_axis',(0.,0.,1.));
#4559=DIRECTION('ref_axis',(1.,0.,0.));
#4560=DIRECTION('',(0.,0.,-1.));
#4561=DIRECTION('center_axis',(0.,0.,1.));
#4562=DIRECTION('ref_axis',(1.,0.,0.));
#4563=DIRECTION('center_axis',(0.,0.,1.));
#4564=DIRECTION('ref_axis',(1.,0.,0.));
#4565=DIRECTION('center_axis',(0.,0.,1.));
#4566=DIRECTION('ref_axis',(1.,0.,0.));
#4567=DIRECTION('center_axis',(0.,0.,1.));
#4568=DIRECTION('ref_axis',(1.,0.,0.));
#4569=DIRECTION('center_axis',(0.,0.,1.));
#4570=DIRECTION('ref_axis',(1.,0.,0.));
#4571=DIRECTION('center_axis',(0.,0.,1.));
#4572=DIRECTION('ref_axis',(1.,0.,0.));
#4573=DIRECTION('center_axis',(0.,0.,1.));
#4574=DIRECTION('ref_axis',(1.,0.,0.));
#4575=DIRECTION('',(0.,0.,-1.));
#4576=DIRECTION('center_axis',(0.,0.,1.));
#4577=DIRECTION('ref_axis',(1.,0.,0.));
#4578=DIRECTION('center_axis',(0.,0.,1.));
#4579=DIRECTION('ref_axis',(1.,0.,0.));
#4580=DIRECTION('center_axis',(0.,0.,1.));
#4581=DIRECTION('ref_axis',(1.,0.,0.));
#4582=DIRECTION('center_axis',(0.,0.,1.));
#4583=DIRECTION('ref_axis',(1.,0.,0.));
#4584=DIRECTION('center_axis',(0.,0.,1.));
#4585=DIRECTION('ref_axis',(1.,0.,0.));
#4586=DIRECTION('',(0.,0.,-1.));
#4587=DIRECTION('center_axis',(0.,0.,1.));
#4588=DIRECTION('ref_axis',(1.,0.,0.));
#4589=DIRECTION('',(0.,0.,-1.));
#4590=DIRECTION('center_axis',(0.,0.,1.));
#4591=DIRECTION('ref_axis',(1.,0.,0.));
#4592=DIRECTION('center_axis',(0.,0.,1.));
#4593=DIRECTION('ref_axis',(1.,0.,0.));
#4594=DIRECTION('axis',(0.,0.,1.));
#4595=DIRECTION('refdir',(1.,0.,0.));
#4596=DIRECTION('axis',(0.,0.,1.));
#4597=DIRECTION('refdir',(1.,0.,0.));
#4598=DIRECTION('center_axis',(0.,1.,0.));
#4599=DIRECTION('ref_axis',(1.,0.,0.));
#4600=DIRECTION('center_axis',(0.,1.,0.));
#4601=DIRECTION('ref_axis',(1.,0.,0.));
#4602=DIRECTION('',(0.,1.,0.));
#4603=DIRECTION('center_axis',(0.,-1.,0.));
#4604=DIRECTION('ref_axis',(1.,0.,0.));
#4605=DIRECTION('center_axis',(0.,-1.,0.));
#4606=DIRECTION('ref_axis',(1.,0.,0.));
#4607=DIRECTION('center_axis',(0.,1.,0.));
#4608=DIRECTION('ref_axis',(1.,0.,0.));
#4609=DIRECTION('center_axis',(0.,1.,0.));
#4610=DIRECTION('ref_axis',(1.,0.,0.));
#4611=DIRECTION('',(0.,1.,0.));
#4612=DIRECTION('center_axis',(0.,-1.,0.));
#4613=DIRECTION('ref_axis',(1.,0.,0.));
#4614=DIRECTION('center_axis',(0.,-1.,0.));
#4615=DIRECTION('ref_axis',(1.,0.,0.));
#4616=DIRECTION('center_axis',(0.,-1.,0.));
#4617=DIRECTION('ref_axis',(1.,0.,0.));
#4618=DIRECTION('center_axis',(0.,1.,0.));
#4619=DIRECTION('ref_axis',(1.,0.,0.));
#4620=DIRECTION('center_axis',(0.,1.,0.));
#4621=DIRECTION('ref_axis',(1.,0.,0.));
#4622=DIRECTION('',(0.,1.,0.));
#4623=DIRECTION('center_axis',(0.,-1.,0.));
#4624=DIRECTION('ref_axis',(1.,0.,0.));
#4625=DIRECTION('center_axis',(0.,-1.,0.));
#4626=DIRECTION('ref_axis',(1.,0.,0.));
#4627=DIRECTION('center_axis',(0.,-1.,0.));
#4628=DIRECTION('ref_axis',(1.,0.,0.));
#4629=DIRECTION('center_axis',(0.,1.,0.));
#4630=DIRECTION('ref_axis',(1.,0.,0.));
#4631=DIRECTION('center_axis',(0.,1.,0.));
#4632=DIRECTION('ref_axis',(1.,0.,0.));
#4633=DIRECTION('',(0.,1.,0.));
#4634=DIRECTION('center_axis',(0.,-1.,0.));
#4635=DIRECTION('ref_axis',(1.,0.,0.));
#4636=DIRECTION('center_axis',(0.,-1.,0.));
#4637=DIRECTION('ref_axis',(1.,0.,0.));
#4638=DIRECTION('center_axis',(0.,1.,0.));
#4639=DIRECTION('ref_axis',(1.,0.,0.));
#4640=DIRECTION('center_axis',(0.,1.,0.));
#4641=DIRECTION('ref_axis',(1.,0.,0.));
#4642=DIRECTION('',(0.,1.,0.));
#4643=DIRECTION('center_axis',(0.,-1.,0.));
#4644=DIRECTION('ref_axis',(1.,0.,0.));
#4645=DIRECTION('center_axis',(0.,-1.,0.));
#4646=DIRECTION('ref_axis',(1.,0.,0.));
#4647=DIRECTION('center_axis',(0.,1.,0.));
#4648=DIRECTION('ref_axis',(1.,0.,0.));
#4649=DIRECTION('center_axis',(0.,1.,0.));
#4650=DIRECTION('ref_axis',(1.,0.,0.));
#4651=DIRECTION('',(0.,1.,0.));
#4652=DIRECTION('center_axis',(0.,-1.,0.));
#4653=DIRECTION('ref_axis',(1.,0.,0.));
#4654=DIRECTION('center_axis',(0.,-1.,0.));
#4655=DIRECTION('ref_axis',(1.,0.,0.));
#4656=DIRECTION('center_axis',(0.,1.,0.));
#4657=DIRECTION('ref_axis',(1.,0.,0.));
#4658=DIRECTION('center_axis',(0.,1.,0.));
#4659=DIRECTION('ref_axis',(1.,0.,0.));
#4660=DIRECTION('',(0.,1.,0.));
#4661=DIRECTION('center_axis',(0.,-1.,0.));
#4662=DIRECTION('ref_axis',(1.,0.,0.));
#4663=DIRECTION('center_axis',(0.,-1.,0.));
#4664=DIRECTION('ref_axis',(1.,0.,0.));
#4665=DIRECTION('center_axis',(0.,-1.,0.));
#4666=DIRECTION('ref_axis',(1.,0.,0.));
#4667=DIRECTION('center_axis',(0.,1.,0.));
#4668=DIRECTION('ref_axis',(1.,0.,0.));
#4669=DIRECTION('center_axis',(0.,1.,0.));
#4670=DIRECTION('ref_axis',(1.,0.,0.));
#4671=DIRECTION('',(0.,1.,0.));
#4672=DIRECTION('center_axis',(0.,-1.,0.));
#4673=DIRECTION('ref_axis',(1.,0.,0.));
#4674=DIRECTION('center_axis',(0.,-1.,0.));
#4675=DIRECTION('ref_axis',(1.,0.,0.));
#4676=DIRECTION('center_axis',(0.,-1.,0.));
#4677=DIRECTION('ref_axis',(1.,0.,0.));
#4678=DIRECTION('center_axis',(0.,1.,0.));
#4679=DIRECTION('ref_axis',(1.,0.,0.));
#4680=DIRECTION('center_axis',(0.,1.,0.));
#4681=DIRECTION('ref_axis',(1.,0.,0.));
#4682=DIRECTION('',(0.,1.,0.));
#4683=DIRECTION('center_axis',(0.,-1.,0.));
#4684=DIRECTION('ref_axis',(1.,0.,0.));
#4685=DIRECTION('center_axis',(0.,-1.,0.));
#4686=DIRECTION('ref_axis',(1.,0.,0.));
#4687=DIRECTION('center_axis',(0.,1.,0.));
#4688=DIRECTION('ref_axis',(1.,0.,0.));
#4689=DIRECTION('center_axis',(0.,1.,0.));
#4690=DIRECTION('ref_axis',(1.,0.,0.));
#4691=DIRECTION('',(0.,1.,0.));
#4692=DIRECTION('center_axis',(0.,-1.,0.));
#4693=DIRECTION('ref_axis',(1.,0.,0.));
#4694=DIRECTION('center_axis',(0.,-1.,0.));
#4695=DIRECTION('ref_axis',(1.,0.,0.));
#4696=DIRECTION('center_axis',(0.,1.,0.));
#4697=DIRECTION('ref_axis',(0.,0.,1.));
#4698=DIRECTION('center_axis',(0.,1.,0.));
#4699=DIRECTION('ref_axis',(0.,0.,-1.));
#4700=DIRECTION('center_axis',(0.,1.,0.));
#4701=DIRECTION('ref_axis',(0.,0.,-1.));
#4702=DIRECTION('center_axis',(0.,1.,0.));
#4703=DIRECTION('ref_axis',(0.,0.,-1.));
#4704=DIRECTION('center_axis',(0.,1.,0.));
#4705=DIRECTION('ref_axis',(0.,0.,-1.));
#4706=DIRECTION('center_axis',(0.,1.,0.));
#4707=DIRECTION('ref_axis',(0.,0.,-1.));
#4708=DIRECTION('center_axis',(0.,1.,0.));
#4709=DIRECTION('ref_axis',(0.,0.,-1.));
#4710=DIRECTION('center_axis',(0.,1.,0.));
#4711=DIRECTION('ref_axis',(0.,0.,-1.));
#4712=DIRECTION('center_axis',(0.,1.,0.));
#4713=DIRECTION('ref_axis',(0.,0.,-1.));
#4714=DIRECTION('center_axis',(0.,1.,0.));
#4715=DIRECTION('ref_axis',(0.,0.,-1.));
#4716=DIRECTION('center_axis',(0.,1.,0.));
#4717=DIRECTION('ref_axis',(0.,0.,-1.));
#4718=DIRECTION('center_axis',(0.,-1.,0.));
#4719=DIRECTION('ref_axis',(1.,0.,0.));
#4720=DIRECTION('center_axis',(0.,-1.,0.));
#4721=DIRECTION('ref_axis',(0.,0.,-1.));
#4722=DIRECTION('center_axis',(0.,-1.,0.));
#4723=DIRECTION('ref_axis',(0.,0.,-1.));
#4724=DIRECTION('center_axis',(0.,-1.,0.));
#4725=DIRECTION('ref_axis',(0.,0.,-1.));
#4726=DIRECTION('center_axis',(0.,-1.,0.));
#4727=DIRECTION('ref_axis',(0.,0.,-1.));
#4728=DIRECTION('center_axis',(0.,-1.,0.));
#4729=DIRECTION('ref_axis',(0.,0.,-1.));
#4730=DIRECTION('center_axis',(0.,-1.,0.));
#4731=DIRECTION('ref_axis',(0.,0.,-1.));
#4732=DIRECTION('center_axis',(0.,-1.,0.));
#4733=DIRECTION('ref_axis',(-1.22464679914735E-16,0.,1.));
#4734=DIRECTION('center_axis',(0.,-1.,0.));
#4735=DIRECTION('ref_axis',(0.,0.,-1.));
#4736=DIRECTION('center_axis',(0.,-1.,0.));
#4737=DIRECTION('ref_axis',(0.,0.,-1.));
#4738=DIRECTION('center_axis',(0.,-1.,0.));
#4739=DIRECTION('ref_axis',(0.,0.,-1.));
#4740=DIRECTION('center_axis',(0.,-1.,0.));
#4741=DIRECTION('ref_axis',(0.,0.,-1.));
#4742=DIRECTION('center_axis',(0.,-1.,0.));
#4743=DIRECTION('ref_axis',(0.,0.,-1.));
#4744=DIRECTION('center_axis',(0.,-1.,0.));
#4745=DIRECTION('ref_axis',(0.,0.,-1.));
#4746=DIRECTION('center_axis',(0.,-1.,0.));
#4747=DIRECTION('ref_axis',(0.,0.,-1.));
#4748=DIRECTION('center_axis',(0.,-1.,0.));
#4749=DIRECTION('ref_axis',(0.,0.,-1.));
#4750=DIRECTION('center_axis',(0.,-1.,0.));
#4751=DIRECTION('ref_axis',(0.,0.,-1.));
#4752=DIRECTION('center_axis',(0.,-1.,0.));
#4753=DIRECTION('ref_axis',(0.,0.,-1.));
#4754=DIRECTION('center_axis',(0.,-1.,0.));
#4755=DIRECTION('ref_axis',(0.,0.,-1.));
#4756=DIRECTION('center_axis',(0.,-1.,0.));
#4757=DIRECTION('ref_axis',(0.,0.,-1.));
#4758=DIRECTION('center_axis',(0.,-1.,0.));
#4759=DIRECTION('ref_axis',(0.,0.,-1.));
#4760=DIRECTION('center_axis',(0.,1.,0.));
#4761=DIRECTION('ref_axis',(0.,0.,1.));
#4762=DIRECTION('center_axis',(0.,-1.,0.));
#4763=DIRECTION('ref_axis',(1.,0.,0.));
#4764=DIRECTION('center_axis',(0.,-1.,0.));
#4765=DIRECTION('ref_axis',(1.,0.,0.));
#4766=DIRECTION('center_axis',(0.,-1.,0.));
#4767=DIRECTION('ref_axis',(1.,0.,0.));
#4768=DIRECTION('',(0.,1.,0.));
#4769=DIRECTION('center_axis',(0.,-1.,0.));
#4770=DIRECTION('ref_axis',(0.,0.,-1.));
#4771=DIRECTION('center_axis',(0.,-1.,0.));
#4772=DIRECTION('ref_axis',(1.,0.,0.));
#4773=DIRECTION('center_axis',(0.,-1.,0.));
#4774=DIRECTION('ref_axis',(1.,0.,0.));
#4775=DIRECTION('',(0.,1.,0.));
#4776=DIRECTION('axis',(0.,0.,1.));
#4777=DIRECTION('refdir',(1.,0.,0.));
#4778=DIRECTION('center_axis',(0.,1.,0.));
#4779=DIRECTION('ref_axis',(1.,0.,0.));
#4780=DIRECTION('center_axis',(0.,1.,0.));
#4781=DIRECTION('ref_axis',(1.,0.,0.));
#4782=DIRECTION('',(0.,1.,0.));
#4783=DIRECTION('center_axis',(0.,-1.,0.));
#4784=DIRECTION('ref_axis',(1.,0.,0.));
#4785=DIRECTION('center_axis',(0.,1.,0.));
#4786=DIRECTION('ref_axis',(1.,0.,0.));
#4787=DIRECTION('center_axis',(0.,1.,0.));
#4788=DIRECTION('ref_axis',(1.,0.,0.));
#4789=DIRECTION('center_axis',(0.,1.,0.));
#4790=DIRECTION('ref_axis',(1.,0.,0.));
#4791=DIRECTION('center_axis',(0.,1.,0.));
#4792=DIRECTION('ref_axis',(1.,0.,0.));
#4793=DIRECTION('',(0.,1.,0.));
#4794=DIRECTION('center_axis',(0.,-1.,0.));
#4795=DIRECTION('ref_axis',(1.,0.,0.));
#4796=DIRECTION('center_axis',(0.,1.,0.));
#4797=DIRECTION('ref_axis',(1.,0.,0.));
#4798=DIRECTION('center_axis',(0.,1.,0.));
#4799=DIRECTION('ref_axis',(1.,0.,0.));
#4800=DIRECTION('center_axis',(0.,1.,0.));
#4801=DIRECTION('ref_axis',(1.,0.,0.));
#4802=DIRECTION('',(0.,1.,0.));
#4803=DIRECTION('center_axis',(0.,-1.,0.));
#4804=DIRECTION('ref_axis',(1.,0.,0.));
#4805=DIRECTION('center_axis',(0.,1.,0.));
#4806=DIRECTION('ref_axis',(1.,0.,0.));
#4807=DIRECTION('center_axis',(0.,1.,0.));
#4808=DIRECTION('ref_axis',(1.,0.,0.));
#4809=DIRECTION('center_axis',(0.,1.,0.));
#4810=DIRECTION('ref_axis',(1.,0.,0.));
#4811=DIRECTION('center_axis',(0.,1.,0.));
#4812=DIRECTION('ref_axis',(1.,0.,0.));
#4813=DIRECTION('center_axis',(0.,1.,0.));
#4814=DIRECTION('ref_axis',(1.,0.,0.));
#4815=DIRECTION('',(0.,1.,0.));
#4816=DIRECTION('center_axis',(0.,-1.,0.));
#4817=DIRECTION('ref_axis',(1.,0.,0.));
#4818=DIRECTION('center_axis',(0.,1.,0.));
#4819=DIRECTION('ref_axis',(1.,0.,0.));
#4820=DIRECTION('center_axis',(0.,1.,0.));
#4821=DIRECTION('ref_axis',(1.,0.,0.));
#4822=DIRECTION('center_axis',(0.,1.,0.));
#4823=DIRECTION('ref_axis',(1.,0.,0.));
#4824=DIRECTION('',(0.,1.,0.));
#4825=DIRECTION('center_axis',(0.,-1.,0.));
#4826=DIRECTION('ref_axis',(1.,0.,0.));
#4827=DIRECTION('center_axis',(0.,1.,0.));
#4828=DIRECTION('ref_axis',(1.,0.,0.));
#4829=DIRECTION('center_axis',(0.,1.,0.));
#4830=DIRECTION('ref_axis',(1.,0.,0.));
#4831=DIRECTION('center_axis',(0.,1.,0.));
#4832=DIRECTION('ref_axis',(1.,0.,0.));
#4833=DIRECTION('',(0.,1.,0.));
#4834=DIRECTION('center_axis',(0.,-1.,0.));
#4835=DIRECTION('ref_axis',(1.,0.,0.));
#4836=DIRECTION('center_axis',(0.,1.,0.));
#4837=DIRECTION('ref_axis',(1.,0.,0.));
#4838=DIRECTION('center_axis',(0.,1.,0.));
#4839=DIRECTION('ref_axis',(1.,0.,0.));
#4840=DIRECTION('center_axis',(0.,1.,0.));
#4841=DIRECTION('ref_axis',(1.,0.,0.));
#4842=DIRECTION('',(0.,1.,0.));
#4843=DIRECTION('center_axis',(0.,-1.,0.));
#4844=DIRECTION('ref_axis',(1.,0.,0.));
#4845=DIRECTION('center_axis',(0.,1.,0.));
#4846=DIRECTION('ref_axis',(1.,0.,0.));
#4847=DIRECTION('center_axis',(0.,1.,0.));
#4848=DIRECTION('ref_axis',(1.,0.,0.));
#4849=DIRECTION('center_axis',(0.,1.,0.));
#4850=DIRECTION('ref_axis',(1.,0.,0.));
#4851=DIRECTION('center_axis',(0.,1.,0.));
#4852=DIRECTION('ref_axis',(1.,0.,0.));
#4853=DIRECTION('',(0.,1.,0.));
#4854=DIRECTION('center_axis',(0.,-1.,0.));
#4855=DIRECTION('ref_axis',(1.,0.,0.));
#4856=DIRECTION('center_axis',(0.,1.,0.));
#4857=DIRECTION('ref_axis',(1.,0.,0.));
#4858=DIRECTION('center_axis',(0.,1.,0.));
#4859=DIRECTION('ref_axis',(1.,0.,0.));
#4860=DIRECTION('center_axis',(0.,1.,0.));
#4861=DIRECTION('ref_axis',(1.,0.,0.));
#4862=DIRECTION('',(0.,1.,0.));
#4863=DIRECTION('center_axis',(0.,-1.,0.));
#4864=DIRECTION('ref_axis',(1.,0.,0.));
#4865=DIRECTION('center_axis',(0.,1.,0.));
#4866=DIRECTION('ref_axis',(1.,0.,0.));
#4867=DIRECTION('center_axis',(0.,1.,0.));
#4868=DIRECTION('ref_axis',(1.,0.,0.));
#4869=DIRECTION('center_axis',(0.,1.,0.));
#4870=DIRECTION('ref_axis',(1.,0.,0.));
#4871=DIRECTION('',(0.,1.,0.));
#4872=DIRECTION('center_axis',(0.,-1.,0.));
#4873=DIRECTION('ref_axis',(1.,0.,0.));
#4874=DIRECTION('center_axis',(0.,1.,0.));
#4875=DIRECTION('ref_axis',(1.,0.,0.));
#4876=DIRECTION('center_axis',(0.,-1.,0.));
#4877=DIRECTION('ref_axis',(0.,0.,-1.));
#4878=DIRECTION('center_axis',(0.,-1.,0.));
#4879=DIRECTION('ref_axis',(0.,0.,-1.));
#4880=DIRECTION('center_axis',(0.,-1.,0.));
#4881=DIRECTION('ref_axis',(0.,0.,-1.));
#4882=DIRECTION('center_axis',(0.,-1.,0.));
#4883=DIRECTION('ref_axis',(0.,0.,-1.));
#4884=DIRECTION('center_axis',(0.,-1.,0.));
#4885=DIRECTION('ref_axis',(0.,0.,-1.));
#4886=DIRECTION('center_axis',(0.,-1.,0.));
#4887=DIRECTION('ref_axis',(0.,0.,-1.));
#4888=DIRECTION('center_axis',(0.,-1.,0.));
#4889=DIRECTION('ref_axis',(0.,0.,-1.));
#4890=DIRECTION('center_axis',(0.,-1.,0.));
#4891=DIRECTION('ref_axis',(0.,0.,-1.));
#4892=DIRECTION('center_axis',(0.,-1.,0.));
#4893=DIRECTION('ref_axis',(0.,0.,-1.));
#4894=DIRECTION('center_axis',(0.,-1.,0.));
#4895=DIRECTION('ref_axis',(0.,0.,-1.));
#4896=DIRECTION('center_axis',(0.,-1.,0.));
#4897=DIRECTION('ref_axis',(0.,0.,-1.));
#4898=DIRECTION('center_axis',(0.,-1.,0.));
#4899=DIRECTION('ref_axis',(1.,0.,0.));
#4900=DIRECTION('center_axis',(0.,-1.,0.));
#4901=DIRECTION('ref_axis',(0.,0.,-1.));
#4902=DIRECTION('center_axis',(0.,1.,0.));
#4903=DIRECTION('ref_axis',(0.,0.,-1.));
#4904=DIRECTION('center_axis',(0.,-1.,0.));
#4905=DIRECTION('ref_axis',(0.,0.,-1.));
#4906=DIRECTION('center_axis',(0.,1.,0.));
#4907=DIRECTION('ref_axis',(0.,0.,-1.));
#4908=DIRECTION('center_axis',(0.,-1.,0.));
#4909=DIRECTION('ref_axis',(0.,0.,-1.));
#4910=DIRECTION('center_axis',(0.,1.,0.));
#4911=DIRECTION('ref_axis',(0.,0.,-1.));
#4912=DIRECTION('center_axis',(0.,-1.,0.));
#4913=DIRECTION('ref_axis',(-1.22464679914735E-16,0.,1.));
#4914=DIRECTION('center_axis',(0.,1.,0.));
#4915=DIRECTION('ref_axis',(0.,0.,-1.));
#4916=DIRECTION('center_axis',(0.,-1.,0.));
#4917=DIRECTION('ref_axis',(0.,0.,-1.));
#4918=DIRECTION('center_axis',(0.,1.,0.));
#4919=DIRECTION('ref_axis',(0.,0.,-1.));
#4920=DIRECTION('center_axis',(0.,-1.,0.));
#4921=DIRECTION('ref_axis',(0.,0.,-1.));
#4922=DIRECTION('center_axis',(0.,1.,0.));
#4923=DIRECTION('ref_axis',(0.,0.,-1.));
#4924=DIRECTION('center_axis',(0.,-1.,0.));
#4925=DIRECTION('ref_axis',(0.,0.,-1.));
#4926=DIRECTION('center_axis',(0.,1.,0.));
#4927=DIRECTION('ref_axis',(0.,0.,-1.));
#4928=DIRECTION('center_axis',(0.,-1.,0.));
#4929=DIRECTION('ref_axis',(0.,0.,-1.));
#4930=DIRECTION('center_axis',(0.,1.,0.));
#4931=DIRECTION('ref_axis',(0.,0.,-1.));
#4932=DIRECTION('center_axis',(0.,-1.,0.));
#4933=DIRECTION('ref_axis',(0.,0.,-1.));
#4934=DIRECTION('center_axis',(0.,1.,0.));
#4935=DIRECTION('ref_axis',(0.,0.,-1.));
#4936=DIRECTION('center_axis',(0.,-1.,0.));
#4937=DIRECTION('ref_axis',(0.,0.,-1.));
#4938=DIRECTION('center_axis',(0.,1.,0.));
#4939=DIRECTION('ref_axis',(0.,0.,-1.));
#4940=DIRECTION('center_axis',(0.,1.,0.));
#4941=DIRECTION('ref_axis',(0.,0.,1.));
#4942=DIRECTION('center_axis',(0.,-1.,0.));
#4943=DIRECTION('ref_axis',(1.,0.,0.));
#4944=DIRECTION('center_axis',(0.,-1.,0.));
#4945=DIRECTION('ref_axis',(1.,0.,0.));
#4946=DIRECTION('center_axis',(0.,-1.,0.));
#4947=DIRECTION('ref_axis',(1.,0.,0.));
#4948=DIRECTION('center_axis',(0.,-1.,0.));
#4949=DIRECTION('ref_axis',(1.,0.,0.));
#4950=DIRECTION('',(0.,1.,0.));
#4951=DIRECTION('center_axis',(0.,-1.,0.));
#4952=DIRECTION('ref_axis',(0.,0.,-1.));
#4953=DIRECTION('center_axis',(0.,-1.,0.));
#4954=DIRECTION('ref_axis',(1.,0.,0.));
#4955=DIRECTION('',(0.,1.,0.));
#4956=DIRECTION('axis',(0.,0.,1.));
#4957=DIRECTION('refdir',(1.,0.,0.));
#4958=DIRECTION('center_axis',(0.,0.,1.));
#4959=DIRECTION('ref_axis',(1.,0.,0.));
#4960=DIRECTION('center_axis',(0.,-1.,0.));
#4961=DIRECTION('ref_axis',(-1.,0.,0.));
#4962=DIRECTION('center_axis',(0.587785252292473,0.,0.809016994374947));
#4963=DIRECTION('ref_axis',(0.809016994374948,0.,-0.587785252292473));
#4964=DIRECTION('center_axis',(0.,-1.,0.));
#4965=DIRECTION('ref_axis',(-0.809016994374948,0.,0.587785252292473));
#4966=DIRECTION('center_axis',(0.951056516295154,0.,0.309016994374948));
#4967=DIRECTION('ref_axis',(0.309016994374947,0.,-0.951056516295154));
#4968=DIRECTION('center_axis',(0.,-1.,0.));
#4969=DIRECTION('ref_axis',(-0.309016994374947,0.,0.951056516295154));
#4970=DIRECTION('center_axis',(0.951056516295154,0.,-0.309016994374948));
#4971=DIRECTION('ref_axis',(-0.309016994374947,0.,-0.951056516295154));
#4972=DIRECTION('center_axis',(0.,-1.,0.));
#4973=DIRECTION('ref_axis',(0.309016994374947,0.,0.951056516295154));
#4974=DIRECTION('center_axis',(0.587785252292473,0.,-0.809016994374948));
#4975=DIRECTION('ref_axis',(-0.809016994374947,0.,-0.587785252292473));
#4976=DIRECTION('center_axis',(0.,-1.,0.));
#4977=DIRECTION('ref_axis',(0.809016994374948,0.,0.587785252292473));
#4978=DIRECTION('center_axis',(0.,0.,-1.));
#4979=DIRECTION('ref_axis',(-1.,0.,-1.22464679914735E-16));
#4980=DIRECTION('center_axis',(0.,-1.,0.));
#4981=DIRECTION('ref_axis',(1.,0.,1.22464679914735E-16));
#4982=DIRECTION('center_axis',(-0.587785252292473,0.,-0.809016994374948));
#4983=DIRECTION('ref_axis',(-0.809016994374947,0.,0.587785252292473));
#4984=DIRECTION('center_axis',(0.,-1.,0.));
#4985=DIRECTION('ref_axis',(0.809016994374948,0.,-0.587785252292473));
#4986=DIRECTION('center_axis',(-0.951056516295154,0.,-0.309016994374948));
#4987=DIRECTION('ref_axis',(-0.309016994374948,0.,0.951056516295154));
#4988=DIRECTION('center_axis',(0.,-1.,0.));
#4989=DIRECTION('ref_axis',(0.309016994374948,0.,-0.951056516295154));
#4990=DIRECTION('center_axis',(-0.951056516295154,0.,0.309016994374948));
#4991=DIRECTION('ref_axis',(0.309016994374947,0.,0.951056516295154));
#4992=DIRECTION('center_axis',(0.,-1.,0.));
#4993=DIRECTION('ref_axis',(-0.309016994374947,0.,-0.951056516295154));
#4994=DIRECTION('center_axis',(-0.587785252292473,0.,0.809016994374948));
#4995=DIRECTION('ref_axis',(0.809016994374947,0.,0.587785252292473));
#4996=DIRECTION('center_axis',(0.,-1.,0.));
#4997=DIRECTION('ref_axis',(-0.809016994374948,0.,-0.587785252292473));
#4998=DIRECTION('',(0.,0.,1.));
#4999=DIRECTION('',(1.,0.,0.));
#5000=DIRECTION('',(0.,0.,1.));
#5001=DIRECTION('',(1.,0.,0.));
#5002=DIRECTION('',(0.,0.,1.));
#5003=DIRECTION('',(1.,0.,0.));
#5004=DIRECTION('axis',(0.,0.,1.));
#5005=DIRECTION('refdir',(1.,0.,0.));
#5006=DIRECTION('center_axis',(0.,1.,0.));
#5007=DIRECTION('ref_axis',(1.,0.,0.));
#5008=DIRECTION('center_axis',(0.,-1.,0.));
#5009=DIRECTION('ref_axis',(1.,0.,0.));
#5010=DIRECTION('',(0.,-1.,0.));
#5011=DIRECTION('center_axis',(0.,-1.,0.));
#5012=DIRECTION('ref_axis',(1.,0.,0.));
#5013=DIRECTION('center_axis',(0.,1.,0.));
#5014=DIRECTION('ref_axis',(1.,0.,0.));
#5015=DIRECTION('center_axis',(0.,1.,0.));
#5016=DIRECTION('ref_axis',(1.,0.,0.));
#5017=DIRECTION('',(0.,-1.,0.));
#5018=DIRECTION('center_axis',(0.,1.,0.));
#5019=DIRECTION('ref_axis',(1.,0.,0.));
#5020=DIRECTION('center_axis',(0.,1.,0.));
#5021=DIRECTION('ref_axis',(1.,0.,0.));
#5022=DIRECTION('center_axis',(0.,1.,0.));
#5023=DIRECTION('ref_axis',(1.,0.,0.));
#5024=DIRECTION('axis',(0.,0.,1.));
#5025=DIRECTION('refdir',(1.,0.,0.));
#5026=DIRECTION('center_axis',(0.,1.,0.));
#5027=DIRECTION('ref_axis',(1.,0.,0.));
#5028=DIRECTION('',(0.866025403784439,-0.5,1.06057523872491E-16));
#5029=DIRECTION('center_axis',(0.,-1.,0.));
#5030=DIRECTION('ref_axis',(1.,0.,0.));
#5031=DIRECTION('center_axis',(0.,-1.,0.));
#5032=DIRECTION('ref_axis',(1.,0.,0.));
#5033=DIRECTION('center_axis',(0.,1.,0.));
#5034=DIRECTION('ref_axis',(1.,0.,0.));
#5035=DIRECTION('',(-0.866025403784439,-0.5,-1.06057523872491E-16));
#5036=DIRECTION('center_axis',(1.4792020664489E-16,0.,-1.));
#5037=DIRECTION('ref_axis',(-1.,0.,-1.4792020664489E-16));
#5038=DIRECTION('',(0.,1.,0.));
#5039=DIRECTION('',(0.,1.,0.));
#5040=DIRECTION('center_axis',(-0.866025403784439,0.,-0.5));
#5041=DIRECTION('ref_axis',(-0.5,0.,0.866025403784439));
#5042=DIRECTION('',(0.,1.,0.));
#5043=DIRECTION('center_axis',(-0.866025403784439,0.,0.5));
#5044=DIRECTION('ref_axis',(0.5,0.,0.866025403784439));
#5045=DIRECTION('',(0.,1.,0.));
#5046=DIRECTION('center_axis',(0.,1.,0.));
#5047=DIRECTION('ref_axis',(1.,0.,0.));
#5048=DIRECTION('center_axis',(0.,1.,0.));
#5049=DIRECTION('ref_axis',(1.,0.,0.));
#5050=DIRECTION('',(0.,-1.,0.));
#5051=DIRECTION('center_axis',(0.,1.,0.));
#5052=DIRECTION('ref_axis',(1.,0.,0.));
#5053=DIRECTION('center_axis',(-2.95840413289779E-16,0.,1.));
#5054=DIRECTION('ref_axis',(1.,0.,2.95840413289779E-16));
#5055=DIRECTION('',(0.,1.,0.));
#5056=DIRECTION('center_axis',(0.866025403784439,0.,-0.5));
#5057=DIRECTION('ref_axis',(-0.5,0.,-0.866025403784439));
#5058=DIRECTION('',(0.,1.,0.));
#5059=DIRECTION('center_axis',(0.866025403784439,0.,0.5));
#5060=DIRECTION('ref_axis',(0.5,0.,-0.866025403784439));
#5061=DIRECTION('center_axis',(0.,1.,0.));
#5062=DIRECTION('ref_axis',(1.,0.,0.));
#5063=DIRECTION('center_axis',(0.,1.,0.));
#5064=DIRECTION('ref_axis',(1.,0.,0.));
#5065=DIRECTION('',(0.,0.,1.));
#5066=DIRECTION('',(1.,0.,0.));
#5067=DIRECTION('',(0.,0.,1.));
#5068=DIRECTION('',(1.,0.,0.));
#5069=DIRECTION('',(0.,-1.,2.22044604925031E-16));
#5070=DIRECTION('',(1.,0.,0.));
#5071=DIRECTION('',(0.,1.,2.22044604925031E-16));
#5072=DIRECTION('',(1.,0.,0.));
#5073=DIRECTION('',(0.,1.,2.22044604925031E-16));
#5074=DIRECTION('',(1.,0.,0.));
#5075=DIRECTION('axis',(0.,0.,1.));
#5076=DIRECTION('refdir',(1.,0.,0.));
#5077=DIRECTION('axis',(0.,0.,1.));
#5078=DIRECTION('refdir',(1.,0.,0.));
#5079=DIRECTION('center_axis',(0.,0.,1.));
#5080=DIRECTION('ref_axis',(1.,0.,0.));
#5081=DIRECTION('center_axis',(0.,0.,1.));
#5082=DIRECTION('ref_axis',(1.,0.,0.));
#5083=DIRECTION('',(0.,0.,1.));
#5084=DIRECTION('center_axis',(0.,0.,-1.));
#5085=DIRECTION('ref_axis',(1.,0.,0.));
#5086=DIRECTION('center_axis',(0.,1.,0.));
#5087=DIRECTION('ref_axis',(1.,0.,0.));
#5088=DIRECTION('center_axis',(0.,-1.,0.));
#5089=DIRECTION('ref_axis',(1.,0.,0.));
#5090=DIRECTION('',(0.,1.,0.));
#5091=DIRECTION('center_axis',(0.,1.,0.));
#5092=DIRECTION('ref_axis',(1.,0.,0.));
#5093=DIRECTION('',(0.,-1.,0.));
#5094=DIRECTION('center_axis',(0.,1.,0.));
#5095=DIRECTION('ref_axis',(1.,0.,0.));
#5096=DIRECTION('',(0.,-1.,0.));
#5097=DIRECTION('center_axis',(0.,-1.,0.));
#5098=DIRECTION('ref_axis',(1.,0.,0.));
#5099=DIRECTION('',(0.,1.,0.));
#5100=DIRECTION('center_axis',(0.,1.,0.));
#5101=DIRECTION('ref_axis',(1.,0.,0.));
#5102=DIRECTION('center_axis',(0.,1.,0.));
#5103=DIRECTION('ref_axis',(-1.,0.,0.));
#5104=DIRECTION('',(-1.,0.,0.));
#5105=DIRECTION('',(0.,0.,1.));
#5106=DIRECTION('',(-1.,0.,0.));
#5107=DIRECTION('',(0.,0.,1.));
#5108=DIRECTION('',(-1.,0.,0.));
#5109=DIRECTION('',(0.,0.,1.));
#5110=DIRECTION('',(-1.,0.,0.));
#5111=DIRECTION('',(0.,0.,-1.));
#5112=DIRECTION('',(-1.,0.,0.));
#5113=DIRECTION('center_axis',(0.,0.,-1.));
#5114=DIRECTION('ref_axis',(-1.,0.,0.));
#5115=DIRECTION('',(1.,0.,0.));
#5116=DIRECTION('',(0.,1.,0.));
#5117=DIRECTION('center_axis',(0.,0.,-1.));
#5118=DIRECTION('ref_axis',(-1.,0.,0.));
#5119=DIRECTION('',(0.,1.,0.));
#5120=DIRECTION('',(1.,0.,0.));
#5121=DIRECTION('center_axis',(0.,-1.,0.));
#5122=DIRECTION('ref_axis',(1.,0.,0.));
#5123=DIRECTION('',(1.,0.,0.));
#5124=DIRECTION('',(0.,0.,1.));
#5125=DIRECTION('',(1.,0.,0.));
#5126=DIRECTION('',(0.,0.,1.));
#5127=DIRECTION('',(1.,0.,0.));
#5128=DIRECTION('',(0.,0.,1.));
#5129=DIRECTION('',(1.,0.,0.));
#5130=DIRECTION('',(0.,0.,-1.));
#5131=DIRECTION('',(1.,0.,0.));
#5132=DIRECTION('center_axis',(0.,0.,-1.));
#5133=DIRECTION('ref_axis',(-1.,0.,0.));
#5134=DIRECTION('',(-1.,0.,0.));
#5135=DIRECTION('',(0.,1.,0.));
#5136=DIRECTION('center_axis',(-1.,0.,0.));
#5137=DIRECTION('ref_axis',(0.,0.,1.));
#5138=DIRECTION('',(0.,-1.,0.));
#5139=DIRECTION('',(0.,0.,-1.));
#5140=DIRECTION('center_axis',(1.,0.,0.));
#5141=DIRECTION('ref_axis',(0.,0.,-1.));
#5142=DIRECTION('',(0.,1.,0.));
#5143=DIRECTION('',(0.,0.,1.));
#5144=DIRECTION('center_axis',(0.,1.,0.));
#5145=DIRECTION('ref_axis',(1.,0.,0.));
#5146=DIRECTION('',(1.,0.,0.));
#5147=DIRECTION('center_axis',(0.,0.,1.));
#5148=DIRECTION('ref_axis',(1.,0.,0.));
#5149=DIRECTION('',(0.,1.,0.));
#5150=DIRECTION('',(0.,1.,0.));
#5151=DIRECTION('',(-1.,0.,0.));
#5152=DIRECTION('',(0.,-1.,0.));
#5153=DIRECTION('',(0.,-1.,0.));
#5154=DIRECTION('center_axis',(0.,1.,0.));
#5155=DIRECTION('ref_axis',(0.,0.,1.));
#5156=DIRECTION('',(-1.,0.,0.));
#5157=DIRECTION('',(0.,0.,1.));
#5158=DIRECTION('',(0.,0.,-1.));
#5159=DIRECTION('center_axis',(1.,0.,0.));
#5160=DIRECTION('ref_axis',(0.,0.,-1.));
#5161=DIRECTION('center_axis',(-1.,0.,0.));
#5162=DIRECTION('ref_axis',(0.,0.,1.));
#5163=DIRECTION('',(0.,1.,0.));
#5164=DIRECTION('center_axis',(0.,0.,-1.));
#5165=DIRECTION('ref_axis',(-1.,0.,0.));
#5166=DIRECTION('center_axis',(1.,0.,0.));
#5167=DIRECTION('ref_axis',(0.,1.,0.));
#5168=DIRECTION('',(0.,1.,0.));
#5169=DIRECTION('center_axis',(-1.,0.,0.));
#5170=DIRECTION('ref_axis',(0.,-1.,0.));
#5171=DIRECTION('',(0.,-1.,0.));
#5172=DIRECTION('center_axis',(0.,0.,1.));
#5173=DIRECTION('ref_axis',(1.,0.,0.));
#5174=DIRECTION('axis',(0.,0.,1.));
#5175=DIRECTION('refdir',(1.,0.,0.));
#5176=DIRECTION('center_axis',(0.,0.,1.));
#5177=DIRECTION('ref_axis',(1.,0.,0.));
#5178=DIRECTION('center_axis',(0.,0.,-1.));
#5179=DIRECTION('ref_axis',(1.,0.,0.));
#5180=DIRECTION('',(0.,0.,-1.));
#5181=DIRECTION('center_axis',(0.,0.,-1.));
#5182=DIRECTION('ref_axis',(1.,0.,0.));
#5183=DIRECTION('center_axis',(0.,0.,1.));
#5184=DIRECTION('ref_axis',(1.,0.,0.));
#5185=DIRECTION('center_axis',(0.,0.,1.));
#5186=DIRECTION('ref_axis',(1.,0.,0.));
#5187=DIRECTION('',(0.,0.,-1.));
#5188=DIRECTION('center_axis',(0.,0.,1.));
#5189=DIRECTION('ref_axis',(1.,0.,0.));
#5190=DIRECTION('center_axis',(0.,0.,1.));
#5191=DIRECTION('ref_axis',(1.,0.,0.));
#5192=DIRECTION('center_axis',(0.,0.,1.));
#5193=DIRECTION('ref_axis',(1.,0.,0.));
#5194=DIRECTION('axis',(0.,0.,1.));
#5195=DIRECTION('refdir',(1.,0.,0.));
#5196=DIRECTION('center_axis',(0.,1.,0.));
#5197=DIRECTION('ref_axis',(1.,0.,0.));
#5198=DIRECTION('center_axis',(0.,1.,0.));
#5199=DIRECTION('ref_axis',(1.,0.,0.));
#5200=DIRECTION('',(0.,1.,0.));
#5201=DIRECTION('center_axis',(0.,-1.,0.));
#5202=DIRECTION('ref_axis',(1.,0.,0.));
#5203=DIRECTION('center_axis',(0.,1.,0.));
#5204=DIRECTION('ref_axis',(1.,0.,0.));
#5205=DIRECTION('center_axis',(0.,1.,0.));
#5206=DIRECTION('ref_axis',(1.,0.,0.));
#5207=DIRECTION('center_axis',(0.,1.,0.));
#5208=DIRECTION('ref_axis',(1.,0.,0.));
#5209=DIRECTION('center_axis',(0.,1.,0.));
#5210=DIRECTION('ref_axis',(1.,0.,0.));
#5211=DIRECTION('center_axis',(0.,1.,0.));
#5212=DIRECTION('ref_axis',(1.,0.,0.));
#5213=DIRECTION('',(0.,-1.,0.));
#5214=DIRECTION('center_axis',(0.,1.,0.));
#5215=DIRECTION('ref_axis',(1.,0.,0.));
#5216=DIRECTION('center_axis',(0.,1.,0.));
#5217=DIRECTION('ref_axis',(1.,0.,0.));
#5218=DIRECTION('center_axis',(0.,1.,0.));
#5219=DIRECTION('ref_axis',(1.,0.,0.));
#5220=DIRECTION('center_axis',(0.,1.,0.));
#5221=DIRECTION('ref_axis',(1.,0.,0.));
#5222=DIRECTION('',(0.,-1.,0.));
#5223=DIRECTION('center_axis',(0.,1.,0.));
#5224=DIRECTION('ref_axis',(1.,0.,0.));
#5225=DIRECTION('axis',(0.,0.,1.));
#5226=DIRECTION('refdir',(1.,0.,0.));
#5227=DIRECTION('center_axis',(0.,1.,0.));
#5228=DIRECTION('ref_axis',(1.,0.,0.));
#5229=DIRECTION('center_axis',(0.,-1.,0.));
#5230=DIRECTION('ref_axis',(1.,0.,0.));
#5231=DIRECTION('',(0.,-1.,0.));
#5232=DIRECTION('center_axis',(0.,-1.,0.));
#5233=DIRECTION('ref_axis',(1.,0.,0.));
#5234=DIRECTION('center_axis',(0.,1.,0.));
#5235=DIRECTION('ref_axis',(1.,0.,0.));
#5236=DIRECTION('center_axis',(0.,1.,0.));
#5237=DIRECTION('ref_axis',(1.,0.,0.));
#5238=DIRECTION('',(0.,-1.,0.));
#5239=DIRECTION('center_axis',(0.,1.,0.));
#5240=DIRECTION('ref_axis',(1.,0.,0.));
#5241=DIRECTION('center_axis',(0.,1.,0.));
#5242=DIRECTION('ref_axis',(1.,0.,0.));
#5243=DIRECTION('center_axis',(0.,1.,0.));
#5244=DIRECTION('ref_axis',(1.,0.,0.));
#5245=DIRECTION('axis',(0.,0.,1.));
#5246=DIRECTION('refdir',(1.,0.,0.));
#5247=DIRECTION('center_axis',(0.,1.,0.));
#5248=DIRECTION('ref_axis',(1.,0.,0.));
#5249=DIRECTION('center_axis',(0.,-1.,0.));
#5250=DIRECTION('ref_axis',(1.,0.,0.));
#5251=DIRECTION('',(0.,-1.,0.));
#5252=DIRECTION('center_axis',(0.,-1.,0.));
#5253=DIRECTION('ref_axis',(1.,0.,0.));
#5254=DIRECTION('center_axis',(0.,1.,0.));
#5255=DIRECTION('ref_axis',(1.,0.,0.));
#5256=DIRECTION('center_axis',(0.,1.,0.));
#5257=DIRECTION('ref_axis',(1.,0.,0.));
#5258=DIRECTION('',(0.,-1.,0.));
#5259=DIRECTION('center_axis',(0.,1.,0.));
#5260=DIRECTION('ref_axis',(1.,0.,0.));
#5261=DIRECTION('center_axis',(0.,1.,0.));
#5262=DIRECTION('ref_axis',(1.,0.,0.));
#5263=DIRECTION('center_axis',(0.,1.,0.));
#5264=DIRECTION('ref_axis',(1.,0.,0.));
#5265=DIRECTION('axis',(0.,0.,1.));
#5266=DIRECTION('refdir',(1.,0.,0.));
#5267=DIRECTION('center_axis',(0.866025403784439,0.,-0.5));
#5268=DIRECTION('ref_axis',(0.5,0.,0.866025403784439));
#5269=DIRECTION('',(-0.5,0.,-0.866025403784439));
#5270=DIRECTION('',(0.,-1.,0.));
#5271=DIRECTION('',(0.5,0.,0.866025403784439));
#5272=DIRECTION('',(0.,-1.,0.));
#5273=DIRECTION('center_axis',(1.60246890531964E-16,0.,-1.));
#5274=DIRECTION('ref_axis',(1.,0.,1.60246890531964E-16));
#5275=DIRECTION('',(-1.,0.,-1.60246890531964E-16));
#5276=DIRECTION('',(0.,-1.,0.));
#5277=DIRECTION('',(1.,0.,1.60246890531964E-16));
#5278=DIRECTION('center_axis',(-0.866025403784439,0.,-0.5));
#5279=DIRECTION('ref_axis',(0.5,0.,-0.866025403784439));
#5280=DIRECTION('',(-0.5,0.,0.866025403784439));
#5281=DIRECTION('',(0.,-1.,0.));
#5282=DIRECTION('',(0.5,0.,-0.866025403784439));
#5283=DIRECTION('center_axis',(-0.866025403784439,0.,0.5));
#5284=DIRECTION('ref_axis',(-0.5,0.,-0.866025403784439));
#5285=DIRECTION('',(0.5,0.,0.866025403784439));
#5286=DIRECTION('',(0.,-1.,0.));
#5287=DIRECTION('',(-0.5,0.,-0.866025403784439));
#5288=DIRECTION('center_axis',(-1.60246890531964E-16,0.,1.));
#5289=DIRECTION('ref_axis',(-1.,0.,-1.60246890531964E-16));
#5290=DIRECTION('',(1.,0.,1.60246890531964E-16));
#5291=DIRECTION('',(0.,-1.,0.));
#5292=DIRECTION('',(-1.,0.,-1.60246890531964E-16));
#5293=DIRECTION('center_axis',(0.866025403784439,0.,0.5));
#5294=DIRECTION('ref_axis',(-0.5,0.,0.866025403784439));
#5295=DIRECTION('',(0.5,0.,-0.866025403784439));
#5296=DIRECTION('',(-0.5,0.,0.866025403784439));
#5297=DIRECTION('center_axis',(0.,1.,0.));
#5298=DIRECTION('ref_axis',(1.,0.,0.));
#5299=DIRECTION('center_axis',(0.,-1.,0.));
#5300=DIRECTION('ref_axis',(0.,0.,-1.));
#5301=DIRECTION('center_axis',(0.,1.,0.));
#5302=DIRECTION('ref_axis',(1.,0.,0.));
#5303=DIRECTION('center_axis',(0.,1.,0.));
#5304=DIRECTION('ref_axis',(1.,0.,0.));
#5305=DIRECTION('center_axis',(0.,1.,0.));
#5306=DIRECTION('ref_axis',(0.,0.,1.));
#5307=DIRECTION('center_axis',(0.,-1.,0.));
#5308=DIRECTION('ref_axis',(1.,0.,0.));
#5309=DIRECTION('center_axis',(0.,-1.,0.));
#5310=DIRECTION('ref_axis',(1.,0.,0.));
#5311=DIRECTION('center_axis',(0.,-1.,0.));
#5312=DIRECTION('ref_axis',(1.,0.,0.));
#5313=DIRECTION('',(0.707106781186547,0.707106781186548,8.65956056235493E-17));
#5314=DIRECTION('center_axis',(0.,-1.,0.));
#5315=DIRECTION('ref_axis',(1.,0.,0.));
#5316=DIRECTION('center_axis',(0.,-1.,0.));
#5317=DIRECTION('ref_axis',(1.,0.,0.));
#5318=DIRECTION('',(0.,1.,0.));
#5319=DIRECTION('center_axis',(0.,1.,0.));
#5320=DIRECTION('ref_axis',(1.,0.,0.));
#5321=DIRECTION('center_axis',(0.,-1.,0.));
#5322=DIRECTION('ref_axis',(1.,0.,0.));
#5323=DIRECTION('',(-0.707106781186547,0.707106781186548,-8.65956056235493E-17));
#5324=DIRECTION('center_axis',(0.,-1.,0.));
#5325=DIRECTION('ref_axis',(0.,0.,-1.));
#5326=DIRECTION('center_axis',(0.,-1.,0.));
#5327=DIRECTION('ref_axis',(1.,0.,0.));
#5328=DIRECTION('center_axis',(0.,1.,0.));
#5329=DIRECTION('ref_axis',(1.,0.,0.));
#5330=DIRECTION('center_axis',(0.,1.,0.));
#5331=DIRECTION('ref_axis',(1.,0.,0.));
#5332=DIRECTION('',(-0.447213595499958,0.894427190999916,-5.47678698264203E-17));
#5333=DIRECTION('center_axis',(0.,-1.,0.));
#5334=DIRECTION('ref_axis',(1.,0.,0.));
#5335=DIRECTION('',(0.,1.,0.));
#5336=DIRECTION('',(0.,0.,1.));
#5337=DIRECTION('',(1.,0.,0.));
#5338=DIRECTION('',(0.,0.,1.));
#5339=DIRECTION('',(1.,0.,0.));
#5340=DIRECTION('',(0.,0.,1.));
#5341=DIRECTION('',(1.,0.,0.));
#5342=DIRECTION('',(0.,0.,1.));
#5343=DIRECTION('',(1.,0.,0.));
#5344=DIRECTION('',(0.,0.,1.));
#5345=DIRECTION('',(1.,0.,0.));
#5346=DIRECTION('',(0.,0.,1.));
#5347=DIRECTION('',(1.,0.,0.));
#5348=DIRECTION('',(0.,0.,1.));
#5349=DIRECTION('',(1.,0.,0.));
#5350=DIRECTION('axis',(0.,0.,1.));
#5351=DIRECTION('refdir',(1.,0.,0.));
#5352=DIRECTION('axis',(0.,0.,1.));
#5353=DIRECTION('refdir',(1.,0.,0.));
#5354=DIRECTION('center_axis',(0.,1.,0.));
#5355=DIRECTION('ref_axis',(1.,0.,0.));
#5356=DIRECTION('center_axis',(0.,1.,0.));
#5357=DIRECTION('ref_axis',(1.,0.,0.));
#5358=DIRECTION('',(0.,1.,0.));
#5359=DIRECTION('center_axis',(0.,-1.,0.));
#5360=DIRECTION('ref_axis',(1.,0.,0.));
#5361=DIRECTION('center_axis',(0.,1.,0.));
#5362=DIRECTION('ref_axis',(1.,0.,0.));
#5363=DIRECTION('center_axis',(0.,1.,0.));
#5364=DIRECTION('ref_axis',(1.,0.,0.));
#5365=DIRECTION('center_axis',(0.,1.,0.));
#5366=DIRECTION('ref_axis',(1.,0.,0.));
#5367=DIRECTION('center_axis',(0.,1.,0.));
#5368=DIRECTION('ref_axis',(1.,0.,0.));
#5369=DIRECTION('',(0.,1.,0.));
#5370=DIRECTION('center_axis',(0.,1.,0.));
#5371=DIRECTION('ref_axis',(1.,0.,0.));
#5372=DIRECTION('center_axis',(0.,1.,0.));
#5373=DIRECTION('ref_axis',(1.,0.,0.));
#5374=DIRECTION('center_axis',(0.,-1.,0.));
#5375=DIRECTION('ref_axis',(1.,0.,0.));
#5376=DIRECTION('center_axis',(0.,1.,0.));
#5377=DIRECTION('ref_axis',(1.,0.,0.));
#5378=DIRECTION('',(0.,1.,0.));
#5379=DIRECTION('center_axis',(0.,1.,0.));
#5380=DIRECTION('ref_axis',(1.,0.,0.));
#5381=DIRECTION('center_axis',(0.,1.,0.));
#5382=DIRECTION('ref_axis',(1.,0.,0.));
#5383=DIRECTION('',(0.,-1.,0.));
#5384=DIRECTION('center_axis',(0.,1.,0.));
#5385=DIRECTION('ref_axis',(1.,0.,0.));
#5386=DIRECTION('center_axis',(0.,1.,0.));
#5387=DIRECTION('ref_axis',(1.,0.,0.));
#5388=DIRECTION('center_axis',(0.,1.,0.));
#5389=DIRECTION('ref_axis',(1.,0.,0.));
#5390=DIRECTION('axis',(0.,0.,1.));
#5391=DIRECTION('refdir',(1.,0.,0.));
#5392=DIRECTION('axis',(0.,0.,1.));
#5393=DIRECTION('refdir',(1.,0.,0.));
#5394=DIRECTION('center_axis',(0.,-1.,0.));
#5395=DIRECTION('ref_axis',(0.,0.,-1.));
#5396=DIRECTION('center_axis',(0.,-1.,0.));
#5397=DIRECTION('ref_axis',(1.,0.,0.));
#5398=DIRECTION('center_axis',(0.,-1.,0.));
#5399=DIRECTION('ref_axis',(1.,0.,0.));
#5400=DIRECTION('center_axis',(1.,0.,1.22464679914735E-16));
#5401=DIRECTION('ref_axis',(-1.22464679914735E-16,0.,1.));
#5402=DIRECTION('center_axis',(0.,1.,0.));
#5403=DIRECTION('ref_axis',(1.,0.,0.));
#5404=DIRECTION('center_axis',(0.,1.,0.));
#5405=DIRECTION('ref_axis',(1.,0.,0.));
#5406=DIRECTION('center_axis',(0.,-1.,0.));
#5407=DIRECTION('ref_axis',(1.,0.,0.));
#5408=DIRECTION('',(0.,1.,0.));
#5409=DIRECTION('center_axis',(0.,-1.,0.));
#5410=DIRECTION('ref_axis',(1.,0.,0.));
#5411=DIRECTION('center_axis',(0.,-1.,0.));
#5412=DIRECTION('ref_axis',(1.,0.,0.));
#5413=DIRECTION('center_axis',(0.,-1.,0.));
#5414=DIRECTION('ref_axis',(1.,0.,0.));
#5415=DIRECTION('',(0.,1.,0.));
#5416=DIRECTION('center_axis',(0.,-1.,0.));
#5417=DIRECTION('ref_axis',(1.,0.,0.));
#5418=DIRECTION('center_axis',(0.,1.,0.));
#5419=DIRECTION('ref_axis',(1.,0.,0.));
#5420=DIRECTION('',(-0.707106781186548,0.707106781186547,-8.65956056235493E-17));
#5421=DIRECTION('center_axis',(0.,-1.,0.));
#5422=DIRECTION('ref_axis',(1.,0.,0.));
#5423=DIRECTION('center_axis',(0.,1.,0.));
#5424=DIRECTION('ref_axis',(0.,0.,1.));
#5425=DIRECTION('center_axis',(0.,-1.,0.));
#5426=DIRECTION('ref_axis',(1.,0.,0.));
#5427=DIRECTION('center_axis',(0.,-1.,0.));
#5428=DIRECTION('ref_axis',(1.,0.,0.));
#5429=DIRECTION('',(0.,1.,0.));
#5430=DIRECTION('center_axis',(0.,-1.,0.));
#5431=DIRECTION('ref_axis',(0.,0.,-1.));
#5432=DIRECTION('center_axis',(0.,-1.,0.));
#5433=DIRECTION('ref_axis',(1.,0.,0.));
#5434=DIRECTION('center_axis',(0.,-1.,0.));
#5435=DIRECTION('ref_axis',(1.,0.,0.));
#5436=DIRECTION('',(0.707106781186548,0.707106781186547,8.65956056235493E-17));
#5437=DIRECTION('axis',(0.,0.,1.));
#5438=DIRECTION('refdir',(1.,0.,0.));
#5439=DIRECTION('center_axis',(0.,-1.,0.));
#5440=DIRECTION('ref_axis',(0.,0.,-1.));
#5441=DIRECTION('center_axis',(0.,-1.,0.));
#5442=DIRECTION('ref_axis',(1.,0.,0.));
#5443=DIRECTION('center_axis',(0.,-1.,0.));
#5444=DIRECTION('ref_axis',(1.,0.,0.));
#5445=DIRECTION('center_axis',(1.,0.,1.22464679914735E-16));
#5446=DIRECTION('ref_axis',(-1.22464679914735E-16,0.,1.));
#5447=DIRECTION('center_axis',(0.,1.,0.));
#5448=DIRECTION('ref_axis',(1.,0.,0.));
#5449=DIRECTION('center_axis',(0.,1.,0.));
#5450=DIRECTION('ref_axis',(1.,0.,0.));
#5451=DIRECTION('center_axis',(0.,-1.,0.));
#5452=DIRECTION('ref_axis',(1.,0.,0.));
#5453=DIRECTION('center_axis',(0.,-1.,0.));
#5454=DIRECTION('ref_axis',(1.,0.,0.));
#5455=DIRECTION('',(0.,1.,0.));
#5456=DIRECTION('center_axis',(0.,1.,0.));
#5457=DIRECTION('ref_axis',(0.,0.,1.));
#5458=DIRECTION('center_axis',(0.,-1.,0.));
#5459=DIRECTION('ref_axis',(1.,0.,0.));
#5460=DIRECTION('center_axis',(0.,-1.,0.));
#5461=DIRECTION('ref_axis',(1.,0.,0.));
#5462=DIRECTION('center_axis',(0.,-1.,0.));
#5463=DIRECTION('ref_axis',(1.,0.,0.));
#5464=DIRECTION('center_axis',(0.,-1.,0.));
#5465=DIRECTION('ref_axis',(1.,0.,0.));
#5466=DIRECTION('',(0.707106781186548,0.707106781186547,8.65956056235494E-17));
#5467=DIRECTION('center_axis',(0.,-1.,0.));
#5468=DIRECTION('ref_axis',(1.,0.,0.));
#5469=DIRECTION('center_axis',(0.,-1.,0.));
#5470=DIRECTION('ref_axis',(1.,0.,0.));
#5471=DIRECTION('',(0.,1.,0.));
#5472=DIRECTION('center_axis',(0.,1.,0.));
#5473=DIRECTION('ref_axis',(1.,0.,0.));
#5474=DIRECTION('center_axis',(0.,-1.,0.));
#5475=DIRECTION('ref_axis',(1.,0.,0.));
#5476=DIRECTION('',(-0.707106781186548,0.707106781186547,-8.65956056235494E-17));
#5477=DIRECTION('center_axis',(0.,-1.,0.));
#5478=DIRECTION('ref_axis',(0.,0.,-1.));
#5479=DIRECTION('center_axis',(0.,-1.,0.));
#5480=DIRECTION('ref_axis',(1.,0.,0.));
#5481=DIRECTION('',(0.,1.,0.));
#5482=DIRECTION('axis',(0.,0.,1.));
#5483=DIRECTION('refdir',(1.,0.,0.));
#5484=DIRECTION('center_axis',(0.,0.,1.));
#5485=DIRECTION('ref_axis',(1.,0.,0.));
#5486=DIRECTION('center_axis',(1.22464679914735E-16,-1.,0.));
#5487=DIRECTION('ref_axis',(-1.,-1.22464679914735E-16,0.));
#5488=DIRECTION('center_axis',(0.78183148246803,0.,0.623489801858733));
#5489=DIRECTION('ref_axis',(0.623489801858734,0.,-0.78183148246803));
#5490=DIRECTION('center_axis',(7.63554790147315E-17,-1.,-9.57467422477103E-17));
#5491=DIRECTION('ref_axis',(-0.623489801858734,-1.22464679914735E-16,0.78183148246803));
#5492=DIRECTION('center_axis',(0.974927912181824,0.,-0.222520933956314));
#5493=DIRECTION('ref_axis',(-0.222520933956314,0.,-0.974927912181824));
#5494=DIRECTION('center_axis',(-2.7250954951288E-17,-1.,-1.19394234705288E-16));
#5495=DIRECTION('ref_axis',(0.222520933956314,-1.22464679914735E-16,0.974927912181824));
#5496=DIRECTION('center_axis',(0.433883739117558,0.,-0.900968867902419));
#5497=DIRECTION('ref_axis',(-0.900968867902419,0.,-0.433883739117558));
#5498=DIRECTION('center_axis',(-1.10336864020811E-16,-1.,-5.31354332312403E-17));
#5499=DIRECTION('ref_axis',(0.900968867902419,-1.22464679914735E-16,0.433883739117558));
#5500=DIRECTION('center_axis',(-0.433883739117558,0.,-0.900968867902419));
#5501=DIRECTION('ref_axis',(-0.900968867902419,0.,0.433883739117558));
#5502=DIRECTION('center_axis',(-1.10336864020811E-16,-1.,5.31354332312403E-17));
#5503=DIRECTION('ref_axis',(0.900968867902419,-1.22464679914735E-16,-0.433883739117558));
#5504=DIRECTION('center_axis',(-0.974927912181824,0.,-0.222520933956314));
#5505=DIRECTION('ref_axis',(-0.222520933956315,0.,0.974927912181824));
#5506=DIRECTION('center_axis',(-2.7250954951288E-17,-1.,1.19394234705288E-16));
#5507=DIRECTION('ref_axis',(0.222520933956315,-1.22464679914735E-16,-0.974927912181824));
#5508=DIRECTION('center_axis',(-0.78183148246803,0.,0.623489801858734));
#5509=DIRECTION('ref_axis',(0.623489801858733,0.,0.78183148246803));
#5510=DIRECTION('center_axis',(7.63554790147315E-17,-1.,9.57467422477103E-17));
#5511=DIRECTION('ref_axis',(-0.623489801858733,-1.22464679914735E-16,-0.78183148246803));
#5512=DIRECTION('axis',(0.,0.,1.));
#5513=DIRECTION('refdir',(1.,0.,0.));
#5514=DIRECTION('center_axis',(0.,0.,1.));
#5515=DIRECTION('ref_axis',(1.,0.,0.));
#5516=DIRECTION('center_axis',(0.,-1.,0.));
#5517=DIRECTION('ref_axis',(0.,0.,-1.));
#5518=DIRECTION('center_axis',(0.,-1.,0.));
#5519=DIRECTION('ref_axis',(0.,0.,-1.));
#5520=DIRECTION('center_axis',(0.,1.,0.));
#5521=DIRECTION('ref_axis',(1.,0.,0.));
#5522=DIRECTION('center_axis',(0.,1.,0.));
#5523=DIRECTION('ref_axis',(1.,0.,0.));
#5524=DIRECTION('center_axis',(0.,1.,0.));
#5525=DIRECTION('ref_axis',(1.,0.,0.));
#5526=DIRECTION('center_axis',(0.,1.,0.));
#5527=DIRECTION('ref_axis',(1.,0.,0.));
#5528=DIRECTION('',(0.,-1.,0.));
#5529=DIRECTION('center_axis',(0.,-1.,0.));
#5530=DIRECTION('ref_axis',(1.,0.,0.));
#5531=DIRECTION('center_axis',(0.,1.,0.));
#5532=DIRECTION('ref_axis',(1.,0.,0.));
#5533=DIRECTION('center_axis',(0.,1.,0.));
#5534=DIRECTION('ref_axis',(1.,0.,0.));
#5535=DIRECTION('center_axis',(0.,1.,0.));
#5536=DIRECTION('ref_axis',(1.,0.,0.));
#5537=DIRECTION('center_axis',(0.,1.,0.));
#5538=DIRECTION('ref_axis',(1.,0.,0.));
#5539=DIRECTION('center_axis',(0.,1.,0.));
#5540=DIRECTION('ref_axis',(1.,0.,0.));
#5541=DIRECTION('center_axis',(0.,1.,0.));
#5542=DIRECTION('ref_axis',(1.,0.,0.));
#5543=DIRECTION('center_axis',(0.,-1.,0.));
#5544=DIRECTION('ref_axis',(1.,0.,0.));
#5545=DIRECTION('center_axis',(0.,-1.,0.));
#5546=DIRECTION('ref_axis',(0.,0.,-1.));
#5547=DIRECTION('center_axis',(8.96625347776458E-17,0.,1.));
#5548=DIRECTION('ref_axis',(1.,0.,0.));
#5549=DIRECTION('center_axis',(0.,-1.,0.));
#5550=DIRECTION('ref_axis',(0.,0.,-1.));
#5551=DIRECTION('center_axis',(0.,1.,0.));
#5552=DIRECTION('ref_axis',(1.,0.,0.));
#5553=DIRECTION('center_axis',(0.,-1.,0.));
#5554=DIRECTION('ref_axis',(1.,0.,0.));
#5555=DIRECTION('center_axis',(0.,-1.,0.));
#5556=DIRECTION('ref_axis',(0.,0.,-1.));
#5557=DIRECTION('center_axis',(0.,0.,1.));
#5558=DIRECTION('ref_axis',(1.,0.,0.));
#5559=DIRECTION('center_axis',(0.,-1.,0.));
#5560=DIRECTION('ref_axis',(0.,0.,-1.));
#5561=DIRECTION('center_axis',(0.,1.,0.));
#5562=DIRECTION('ref_axis',(1.,0.,0.));
#5563=DIRECTION('center_axis',(0.,-1.,0.));
#5564=DIRECTION('ref_axis',(1.,0.,0.));
#5565=DIRECTION('center_axis',(0.,-1.,0.));
#5566=DIRECTION('ref_axis',(1.,0.,0.));
#5567=DIRECTION('center_axis',(0.,-1.,0.));
#5568=DIRECTION('ref_axis',(0.,0.,-1.));
#5569=DIRECTION('center_axis',(0.,0.,1.));
#5570=DIRECTION('ref_axis',(1.,0.,0.));
#5571=DIRECTION('center_axis',(0.,-1.,0.));
#5572=DIRECTION('ref_axis',(0.,0.,-1.));
#5573=DIRECTION('center_axis',(0.,1.,0.));
#5574=DIRECTION('ref_axis',(1.,0.,0.));
#5575=DIRECTION('center_axis',(0.,-1.,0.));
#5576=DIRECTION('ref_axis',(1.,0.,0.));
#5577=DIRECTION('center_axis',(0.,-1.,0.));
#5578=DIRECTION('ref_axis',(0.,0.,-1.));
#5579=DIRECTION('center_axis',(8.96625347776458E-17,0.,1.));
#5580=DIRECTION('ref_axis',(1.,0.,0.));
#5581=DIRECTION('center_axis',(0.,-1.,0.));
#5582=DIRECTION('ref_axis',(0.,0.,-1.));
#5583=DIRECTION('center_axis',(0.,1.,0.));
#5584=DIRECTION('ref_axis',(1.,0.,0.));
#5585=DIRECTION('center_axis',(0.,-1.,0.));
#5586=DIRECTION('ref_axis',(1.,0.,0.));
#5587=DIRECTION('center_axis',(0.,-1.,0.));
#5588=DIRECTION('ref_axis',(0.,0.,-1.));
#5589=DIRECTION('center_axis',(0.,0.,1.));
#5590=DIRECTION('ref_axis',(1.,0.,0.));
#5591=DIRECTION('center_axis',(0.,-1.,0.));
#5592=DIRECTION('ref_axis',(0.,0.,-1.));
#5593=DIRECTION('center_axis',(0.,1.,0.));
#5594=DIRECTION('ref_axis',(1.,0.,0.));
#5595=DIRECTION('center_axis',(0.,1.,0.));
#5596=DIRECTION('ref_axis',(1.,0.,0.));
#5597=DIRECTION('',(0.,1.,0.));
#5598=DIRECTION('center_axis',(0.,-1.,0.));
#5599=DIRECTION('ref_axis',(1.,0.,0.));
#5600=DIRECTION('center_axis',(0.,-1.,0.));
#5601=DIRECTION('ref_axis',(1.,0.,0.));
#5602=DIRECTION('center_axis',(0.,1.,0.));
#5603=DIRECTION('ref_axis',(1.,0.,0.));
#5604=DIRECTION('center_axis',(0.,-1.,0.));
#5605=DIRECTION('ref_axis',(0.,0.,-1.));
#5606=DIRECTION('center_axis',(0.,0.,1.));
#5607=DIRECTION('ref_axis',(1.,0.,0.));
#5608=DIRECTION('center_axis',(0.,-1.,0.));
#5609=DIRECTION('ref_axis',(0.,0.,-1.));
#5610=DIRECTION('center_axis',(0.,-1.,0.));
#5611=DIRECTION('ref_axis',(-1.,0.,0.));
#5612=DIRECTION('center_axis',(0.,1.,0.));
#5613=DIRECTION('ref_axis',(1.,0.,0.));
#5614=DIRECTION('axis',(0.,0.,1.));
#5615=DIRECTION('refdir',(1.,0.,0.));
#5616=DIRECTION('center_axis',(0.,1.,0.));
#5617=DIRECTION('ref_axis',(0.,0.,1.));
#5618=DIRECTION('center_axis',(0.,-1.,0.));
#5619=DIRECTION('ref_axis',(1.,0.,0.));
#5620=DIRECTION('center_axis',(0.,-1.,0.));
#5621=DIRECTION('ref_axis',(1.,0.,0.));
#5622=DIRECTION('center_axis',(0.,-1.,0.));
#5623=DIRECTION('ref_axis',(1.,0.,0.));
#5624=DIRECTION('center_axis',(0.,-1.,0.));
#5625=DIRECTION('ref_axis',(1.,0.,0.));
#5626=DIRECTION('',(0.,1.,0.));
#5627=DIRECTION('center_axis',(0.,-1.,0.));
#5628=DIRECTION('ref_axis',(0.,0.,-1.));
#5629=DIRECTION('center_axis',(0.,-1.,0.));
#5630=DIRECTION('ref_axis',(1.,0.,0.));
#5631=DIRECTION('center_axis',(0.,-1.,0.));
#5632=DIRECTION('ref_axis',(1.,0.,0.));
#5633=DIRECTION('',(0.,1.,0.));
#5634=DIRECTION('center_axis',(0.,1.,0.));
#5635=DIRECTION('ref_axis',(0.,0.,1.));
#5636=DIRECTION('center_axis',(0.,-1.,0.));
#5637=DIRECTION('ref_axis',(1.,0.,0.));
#5638=DIRECTION('center_axis',(0.,-1.,0.));
#5639=DIRECTION('ref_axis',(1.,0.,0.));
#5640=DIRECTION('center_axis',(0.,-1.,0.));
#5641=DIRECTION('ref_axis',(1.,0.,0.));
#5642=DIRECTION('center_axis',(0.,-1.,0.));
#5643=DIRECTION('ref_axis',(1.,0.,0.));
#5644=DIRECTION('',(0.,1.,0.));
#5645=DIRECTION('center_axis',(0.,-1.,0.));
#5646=DIRECTION('ref_axis',(0.,0.,-1.));
#5647=DIRECTION('center_axis',(0.,-1.,0.));
#5648=DIRECTION('ref_axis',(1.,0.,0.));
#5649=DIRECTION('center_axis',(0.,-1.,0.));
#5650=DIRECTION('ref_axis',(1.,0.,0.));
#5651=DIRECTION('',(0.,1.,0.));
#5652=DIRECTION('',(0.,0.,1.));
#5653=DIRECTION('',(1.,0.,0.));
#5654=DIRECTION('',(0.,0.,1.));
#5655=DIRECTION('',(1.,0.,0.));
#5656=DIRECTION('',(0.,0.,1.));
#5657=DIRECTION('',(1.,0.,0.));
#5658=DIRECTION('',(0.,0.,1.));
#5659=DIRECTION('',(1.,0.,0.));
#5660=DIRECTION('',(0.,0.,1.));
#5661=DIRECTION('',(1.,0.,0.));
#5662=DIRECTION('axis',(0.,0.,1.));
#5663=DIRECTION('refdir',(1.,0.,0.));
#5664=DIRECTION('center_axis',(0.,1.,0.));
#5665=DIRECTION('ref_axis',(1.,0.,0.));
#5666=DIRECTION('center_axis',(0.,-1.,0.));
#5667=DIRECTION('ref_axis',(1.,0.,0.));
#5668=DIRECTION('',(0.,-1.,0.));
#5669=DIRECTION('center_axis',(0.,-1.,0.));
#5670=DIRECTION('ref_axis',(1.,0.,0.));
#5671=DIRECTION('center_axis',(0.,1.,0.));
#5672=DIRECTION('ref_axis',(1.,0.,0.));
#5673=DIRECTION('center_axis',(0.,1.,0.));
#5674=DIRECTION('ref_axis',(1.,0.,0.));
#5675=DIRECTION('',(0.,-1.,0.));
#5676=DIRECTION('center_axis',(0.,1.,0.));
#5677=DIRECTION('ref_axis',(1.,0.,0.));
#5678=DIRECTION('center_axis',(0.,1.,0.));
#5679=DIRECTION('ref_axis',(1.,0.,0.));
#5680=DIRECTION('center_axis',(0.,1.,0.));
#5681=DIRECTION('ref_axis',(1.,0.,0.));
#5682=DIRECTION('',(0.,0.,1.));
#5683=DIRECTION('',(1.,0.,0.));
#5684=DIRECTION('',(0.,0.,1.));
#5685=DIRECTION('',(1.,0.,0.));
#5686=DIRECTION('',(0.,0.,1.));
#5687=DIRECTION('',(1.,0.,0.));
#5688=DIRECTION('',(0.,0.,1.));
#5689=DIRECTION('',(1.,0.,0.));
#5690=DIRECTION('',(0.,0.,1.));
#5691=DIRECTION('',(1.,0.,0.));
#5692=DIRECTION('',(0.,0.,1.));
#5693=DIRECTION('',(1.,0.,0.));
#5694=DIRECTION('',(0.,0.,1.));
#5695=DIRECTION('',(1.,0.,0.));
#5696=DIRECTION('',(0.,0.,1.));
#5697=DIRECTION('',(1.,0.,0.));
#5698=CARTESIAN_POINT('',(0.,0.,0.));
#5699=CARTESIAN_POINT('',(0.,0.,0.));
#5700=CARTESIAN_POINT('',(0.,0.,0.));
#5701=CARTESIAN_POINT('Origin',(-2.,0.,10.1));
#5702=CARTESIAN_POINT('',(-2.75,-9.18485099360515E-17,10.2));
#5703=CARTESIAN_POINT('Origin',(-2.,0.,10.2));
#5704=CARTESIAN_POINT('',(-2.75,9.18485099360515E-17,11.));
#5705=CARTESIAN_POINT('',(-2.75,-9.18485099360515E-17,10.1));
#5706=CARTESIAN_POINT('Origin',(-2.,0.,11.));
#5707=CARTESIAN_POINT('Origin',(2.,-3.,10.1));
#5708=CARTESIAN_POINT('',(1.575,-3.,10.2));
#5709=CARTESIAN_POINT('Origin',(2.,-3.,10.2));
#5710=CARTESIAN_POINT('',(1.575,-3.,11.));
#5711=CARTESIAN_POINT('',(1.575,-3.,10.1));
#5712=CARTESIAN_POINT('Origin',(2.,-3.,11.));
#5713=CARTESIAN_POINT('Origin',(-6.,3.,10.1));
#5714=CARTESIAN_POINT('',(-6.425,3.,10.2));
#5715=CARTESIAN_POINT('Origin',(-6.,3.,10.2));
#5716=CARTESIAN_POINT('',(-6.425,3.,11.));
#5717=CARTESIAN_POINT('',(-6.425,3.,10.1));
#5718=CARTESIAN_POINT('Origin',(-6.,3.,11.));
#5719=CARTESIAN_POINT('Origin',(-6.,-3.,10.1));
#5720=CARTESIAN_POINT('',(-6.425,-3.,10.2));
#5721=CARTESIAN_POINT('Origin',(-6.,-3.,10.2));
#5722=CARTESIAN_POINT('',(-6.425,-3.,11.));
#5723=CARTESIAN_POINT('',(-6.425,-3.,10.1));
#5724=CARTESIAN_POINT('Origin',(-6.,-3.,11.));
#5725=CARTESIAN_POINT('Origin',(2.,3.,10.1));
#5726=CARTESIAN_POINT('',(1.575,3.,10.2));
#5727=CARTESIAN_POINT('Origin',(2.,3.,10.2));
#5728=CARTESIAN_POINT('',(1.575,3.,11.));
#5729=CARTESIAN_POINT('',(1.575,3.,10.1));
#5730=CARTESIAN_POINT('Origin',(2.,3.,11.));
#5731=CARTESIAN_POINT('Origin',(3.,4.,10.2));
#5732=CARTESIAN_POINT('',(3.,4.,10.2));
#5733=CARTESIAN_POINT('',(-7.,4.,10.2));
#5734=CARTESIAN_POINT('',(3.,4.,10.2));
#5735=CARTESIAN_POINT('',(-7.,4.,11.));
#5736=CARTESIAN_POINT('',(-7.,4.,10.2));
#5737=CARTESIAN_POINT('',(3.,4.,11.));
#5738=CARTESIAN_POINT('',(3.,4.,11.));
#5739=CARTESIAN_POINT('',(3.,4.,10.2));
#5740=CARTESIAN_POINT('Origin',(3.,-4.,10.2));
#5741=CARTESIAN_POINT('',(3.,-4.,10.2));
#5742=CARTESIAN_POINT('',(3.,-4.,10.2));
#5743=CARTESIAN_POINT('',(3.,-4.,11.));
#5744=CARTESIAN_POINT('',(3.,-4.,11.));
#5745=CARTESIAN_POINT('',(3.,-4.,10.2));
#5746=CARTESIAN_POINT('Origin',(-7.,-4.,10.2));
#5747=CARTESIAN_POINT('',(-7.,-4.,10.2));
#5748=CARTESIAN_POINT('',(-7.,-4.,10.2));
#5749=CARTESIAN_POINT('',(-7.,-4.,11.));
#5750=CARTESIAN_POINT('',(-7.,-4.,11.));
#5751=CARTESIAN_POINT('',(-7.,-4.,10.2));
#5752=CARTESIAN_POINT('Origin',(-7.,4.,10.2));
#5753=CARTESIAN_POINT('',(-7.,4.,10.2));
#5754=CARTESIAN_POINT('',(-7.,4.,11.));
#5755=CARTESIAN_POINT('Origin',(-2.,0.,11.));
#5756=CARTESIAN_POINT('Origin',(-2.,0.,10.2));
#5757=CARTESIAN_POINT('',(0.,0.,0.));
#5758=CARTESIAN_POINT('Origin',(-2.,0.,7.5));
#5759=CARTESIAN_POINT('',(-2.4,-4.89858719658941E-17,8.5));
#5760=CARTESIAN_POINT('Origin',(-2.,0.,8.5));
#5761=CARTESIAN_POINT('',(-2.4,-4.89858719658941E-17,7.5));
#5762=CARTESIAN_POINT('',(-2.4,-4.89858719658941E-17,7.5));
#5763=CARTESIAN_POINT('Origin',(-2.,0.,7.5));
#5764=CARTESIAN_POINT('Origin',(-2.,0.,7.5));
#5765=CARTESIAN_POINT('Origin',(-2.,0.,11.));
#5766=CARTESIAN_POINT('',(-3.2,-1.46957615897682E-16,11.));
#5767=CARTESIAN_POINT('Origin',(-2.,0.,11.));
#5768=CARTESIAN_POINT('',(-2.75,-9.18485099360515E-17,11.));
#5769=CARTESIAN_POINT('Origin',(-2.,0.,11.));
#5770=CARTESIAN_POINT('Origin',(-2.,0.,11.));
#5771=CARTESIAN_POINT('',(-3.2,-1.46957615897682E-16,11.4));
#5772=CARTESIAN_POINT('Origin',(-2.,0.,11.4));
#5773=CARTESIAN_POINT('',(-3.2,-1.46957615897682E-16,11.));
#5774=CARTESIAN_POINT('Origin',(-2.,0.,11.4));
#5775=CARTESIAN_POINT('Origin',(-2.,0.,9.3));
#5776=CARTESIAN_POINT('',(-2.75,-9.18485099360515E-17,9.3));
#5777=CARTESIAN_POINT('Origin',(-2.,0.,9.3));
#5778=CARTESIAN_POINT('',(-2.6,-7.34788079488412E-17,9.3));
#5779=CARTESIAN_POINT('Origin',(-2.,0.,9.3));
#5780=CARTESIAN_POINT('Origin',(-2.,0.,9.3));
#5781=CARTESIAN_POINT('',(-2.75,-9.18485099360515E-17,9.3));
#5782=CARTESIAN_POINT('Origin',(-2.,0.,8.5));
#5783=CARTESIAN_POINT('',(-2.6,-7.34788079488412E-17,8.5));
#5784=CARTESIAN_POINT('',(-2.6,-7.34788079488412E-17,8.5));
#5785=CARTESIAN_POINT('Origin',(-2.,0.,8.5));
#5786=CARTESIAN_POINT('Origin',(-2.,0.,8.5));
#5787=CARTESIAN_POINT('',(0.,0.,0.));
#5788=CARTESIAN_POINT('',(0.,0.,0.));
#5789=CARTESIAN_POINT('Origin',(0.339918693812442,0.,-1.04616216792467));
#5790=CARTESIAN_POINT('',(0.119918693812442,0.,-1.04616216792467));
#5791=CARTESIAN_POINT('Origin',(0.339918693812442,0.,-1.04616216792467));
#5792=CARTESIAN_POINT('',(0.119918693812442,0.247376716776579,-1.04616216792467));
#5793=CARTESIAN_POINT('',(0.119918693812442,0.,-1.04616216792467));
#5794=CARTESIAN_POINT('',(0.174765758038764,0.35,-0.900819442598166));
#5795=CARTESIAN_POINT('Ctrl Pts',(0.174765758038763,0.35,-0.900819442598166));
#5796=CARTESIAN_POINT('Ctrl Pts',(0.16615910126156,0.335479408675346,-0.910599186515576));
#5797=CARTESIAN_POINT('Ctrl Pts',(0.157611943697822,0.321649098925924,-0.922105787154342));
#5798=CARTESIAN_POINT('Ctrl Pts',(0.142410854924046,0.296417377297428,-0.948090475176036));
#5799=CARTESIAN_POINT('Ctrl Pts',(0.135635598256597,0.284856881183445,-0.962749516762522));
#5800=CARTESIAN_POINT('Ctrl Pts',(0.124807600924644,0.264292426692751,-0.996493855518017));
#5801=CARTESIAN_POINT('Ctrl Pts',(0.12107905659851,0.255687624123886,-1.01568738120414));
#5802=CARTESIAN_POINT('Ctrl Pts',(0.119995150322276,0.24900173289775,-1.03947451044843));
#5803=CARTESIAN_POINT('Ctrl Pts',(0.119918693812442,0.248148180937244,-1.04281359823645));
#5804=CARTESIAN_POINT('Ctrl Pts',(0.119918693812442,0.247376716776579,-1.04616216792467));
#5805=CARTESIAN_POINT('',(0.388099915049348,0.35,-0.831502973106184));
#5806=CARTESIAN_POINT('Origin',(0.339918693812442,0.35,-1.04616216792467));
#5807=CARTESIAN_POINT('',(0.52031818912536,0.35,-1.17208286555157));
#5808=CARTESIAN_POINT('Ctrl Pts',(0.52031818912536,0.35,-1.17208286555157));
#5809=CARTESIAN_POINT('Ctrl Pts',(0.529217457694123,0.335332571878444,-1.15933338442007));
#5810=CARTESIAN_POINT('Ctrl Pts',(0.537396458457103,0.321517770338583,-1.14467059284705));
#5811=CARTESIAN_POINT('Ctrl Pts',(0.550248212225112,0.296532793702566,-1.11286085586034));
#5812=CARTESIAN_POINT('Ctrl Pts',(0.555078018641098,0.285216775966753,-1.09565550010774));
#5813=CARTESIAN_POINT('Ctrl Pts',(0.560591549482129,0.264680669899339,-1.05711602071761));
#5814=CARTESIAN_POINT('Ctrl Pts',(0.56078880978987,0.255831783241444,-1.03561092919333));
#5815=CARTESIAN_POINT('Ctrl Pts',(0.554627960771623,0.244745328150165,-0.994433608378458));
#5816=CARTESIAN_POINT('Ctrl Pts',(0.549175023311742,0.241941375180247,-0.975354466173215));
#5817=CARTESIAN_POINT('Ctrl Pts',(0.532711855060331,0.242062069598183,-0.938206075044727));
#5818=CARTESIAN_POINT('Ctrl Pts',(0.521946739366384,0.245143826724661,-0.921041750757787));
#5819=CARTESIAN_POINT('Ctrl Pts',(0.494476822014916,0.25808943656053,-0.887869891643464));
#5820=CARTESIAN_POINT('Ctrl Pts',(0.477731860324512,0.268767859044401,-0.873445791067852));
#5821=CARTESIAN_POINT('Ctrl Pts',(0.43505445349855,0.301421636034264,-0.84547220309525));
#5822=CARTESIAN_POINT('Ctrl Pts',(0.409474560891576,0.32558298615786,-0.836300608451158));
#5823=CARTESIAN_POINT('Ctrl Pts',(0.388099915049348,0.35,-0.831502973106184));
#5824=CARTESIAN_POINT('',(0.267986765351098,0.35,-1.25407031511432));
#5825=CARTESIAN_POINT('Origin',(0.339918693812442,0.35,-1.04616216792467));
#5826=CARTESIAN_POINT('Ctrl Pts',(0.119918693812442,0.247376716776579,-1.04616216792467));
#5827=CARTESIAN_POINT('Ctrl Pts',(0.119918693812442,0.243706481856949,-1.0620929629339));
#5828=CARTESIAN_POINT('Ctrl Pts',(0.121649354618456,0.241892736284291,-1.07823803146977));
#5829=CARTESIAN_POINT('Ctrl Pts',(0.129925208402574,0.242150819014083,-1.11515786183808));
#5830=CARTESIAN_POINT('Ctrl Pts',(0.137545730009388,0.245541115579871,-1.13486353269143));
#5831=CARTESIAN_POINT('Ctrl Pts',(0.159894075495139,0.25896926022056,-1.17516872094799));
#5832=CARTESIAN_POINT('Ctrl Pts',(0.175488151194729,0.270150443771654,-1.19412647612185));
#5833=CARTESIAN_POINT('Ctrl Pts',(0.216960528286492,0.30273418323525,-1.2315190249125));
#5834=CARTESIAN_POINT('Ctrl Pts',(0.243776713476771,0.325833097600423,-1.24569413677302));
#5835=CARTESIAN_POINT('Ctrl Pts',(0.267986765351098,0.35,-1.25407031511432));
#5836=CARTESIAN_POINT('Origin',(-0.889918693812442,0.,-0.64656377752172));
#5837=CARTESIAN_POINT('',(-1.10991869381244,0.,-0.64656377752172));
#5838=CARTESIAN_POINT('Origin',(-0.889918693812442,0.,-0.64656377752172));
#5839=CARTESIAN_POINT('',(-1.10991869381244,0.35,-0.64656377752172));
#5840=CARTESIAN_POINT('',(-1.10991869381244,0.,-0.64656377752172));
#5841=CARTESIAN_POINT('',(-1.10987928032073,0.35,-0.642399598979491));
#5842=CARTESIAN_POINT('Origin',(-0.889918693812442,0.35,-0.64656377752172));
#5843=CARTESIAN_POINT('',(-0.802724611619556,0.35,-0.444580629634229));
#5844=CARTESIAN_POINT('Ctrl Pts',(-0.802724611619556,0.35,-0.444580629634229));
#5845=CARTESIAN_POINT('Ctrl Pts',(-0.814693298418458,0.335469703254327,
-0.439413868588076));
#5846=CARTESIAN_POINT('Ctrl Pts',(-0.828288194978147,0.321630486900879,
-0.43483810386629));
#5847=CARTESIAN_POINT('Ctrl Pts',(-0.857626293279467,0.296466623645907,
-0.42843076421223));
#5848=CARTESIAN_POINT('Ctrl Pts',(-0.873562500583475,0.284968850954313,
-0.426522755127025));
#5849=CARTESIAN_POINT('Ctrl Pts',(-0.908944175205009,0.264389371081104,
-0.426610046318699));
#5850=CARTESIAN_POINT('Ctrl Pts',(-0.92841189425645,0.255739222721824,-0.428985062409478));
#5851=CARTESIAN_POINT('Ctrl Pts',(-0.966701070362238,0.244572490203357,
-0.439509162402781));
#5852=CARTESIAN_POINT('Ctrl Pts',(-0.984800606765884,0.24187970665778,-0.447081989738821));
#5853=CARTESIAN_POINT('Ctrl Pts',(-1.02033222655978,0.242137933247099,-0.468098181585364));
#5854=CARTESIAN_POINT('Ctrl Pts',(-1.03672671564999,0.245516880218307,-0.48142671327546));
#5855=CARTESIAN_POINT('Ctrl Pts',(-1.0681914718434,0.258930838869848,-0.515141616697553));
#5856=CARTESIAN_POINT('Ctrl Pts',(-1.08142350523446,0.270117119131826,-0.535848665318461));
#5857=CARTESIAN_POINT('Ctrl Pts',(-1.10419503710794,0.302714929726701,-0.586877157140458));
#5858=CARTESIAN_POINT('Ctrl Pts',(-1.10939416747485,0.325822565838319,-0.616774927746324));
#5859=CARTESIAN_POINT('Ctrl Pts',(-1.10987928032073,0.35,-0.642399598979491));
#5860=CARTESIAN_POINT('',(-0.670876851625708,0.35,-0.626053502744384));
#5861=CARTESIAN_POINT('Origin',(-0.889918693812442,0.35,-0.64656377752172));
#5862=CARTESIAN_POINT('',(-0.953929883998579,0.35,-0.857045528585688));
#5863=CARTESIAN_POINT('Ctrl Pts',(-0.95392988399858,0.35,-0.857045528585688));
#5864=CARTESIAN_POINT('Ctrl Pts',(-0.939113614143974,0.335390975831829,
-0.861551415973636));
#5865=CARTESIAN_POINT('Ctrl Pts',(-0.922713318211477,0.32162844535795,-0.864791301338213));
#5866=CARTESIAN_POINT('Ctrl Pts',(-0.888689691679126,0.296761201350329,
-0.867202773669637));
#5867=CARTESIAN_POINT('Ctrl Pts',(-0.870968703349679,0.285505993520706,
-0.866515344265356));
#5868=CARTESIAN_POINT('Ctrl Pts',(-0.832657955828336,0.264913063744833,
-0.859966994580057));
#5869=CARTESIAN_POINT('Ctrl Pts',(-0.812042610895507,0.255983013500831,
-0.853529132681505));
#5870=CARTESIAN_POINT('Ctrl Pts',(-0.774637004578397,0.244799211872409,
-0.834944631013121));
#5871=CARTESIAN_POINT('Ctrl Pts',(-0.758129671802899,0.241962745238242,
-0.823863745365518));
#5872=CARTESIAN_POINT('Ctrl Pts',(-0.72783201892456,0.242038904448235,-0.796734896229851));
#5873=CARTESIAN_POINT('Ctrl Pts',(-0.714819045120535,0.245095813663096,
-0.781209421868766));
#5874=CARTESIAN_POINT('Ctrl Pts',(-0.691707150272296,0.257996207173294,
-0.744838566725142));
#5875=CARTESIAN_POINT('Ctrl Pts',(-0.683135660593065,0.268662345405233,
-0.72444259762104));
#5876=CARTESIAN_POINT('Ctrl Pts',(-0.66965672580744,0.301328368152827,-0.675132080669759));
#5877=CARTESIAN_POINT('Ctrl Pts',(-0.668830436944159,0.325533869830935,
-0.647908424074828));
#5878=CARTESIAN_POINT('Ctrl Pts',(-0.670876851625708,0.35,-0.626053502744384));
#5879=CARTESIAN_POINT('Origin',(-0.889918693812442,0.35,-0.64656377752172));
#5880=CARTESIAN_POINT('Origin',(1.1,0.,0.));
#5881=CARTESIAN_POINT('',(0.88,0.,2.69422295812418E-17));
#5882=CARTESIAN_POINT('Origin',(1.1,0.,0.));
#5883=CARTESIAN_POINT('',(0.88,0.35,2.69422295812418E-17));
#5884=CARTESIAN_POINT('',(0.88,0.,2.69422295812418E-17));
#5885=CARTESIAN_POINT('',(0.910735790157152,0.35,0.112156403618172));
#5886=CARTESIAN_POINT('Origin',(1.1,0.35,0.));
#5887=CARTESIAN_POINT('',(1.27550420984285,0.35,0.132658480043447));
#5888=CARTESIAN_POINT('Ctrl Pts',(1.27550420984285,0.35,0.132658480043447));
#5889=CARTESIAN_POINT('Ctrl Pts',(1.26611782177473,0.33531546276274,0.145076462072449));
#5890=CARTESIAN_POINT('Ctrl Pts',(1.25468431627751,0.321485352158938,0.157400492027332));
#5891=CARTESIAN_POINT('Ctrl Pts',(1.22835219222699,0.296466041103173,0.179483010322184));
#5892=CARTESIAN_POINT('Ctrl Pts',(1.21344338101808,0.285132356747975,0.189407731207313));
#5893=CARTESIAN_POINT('Ctrl Pts',(1.17846267135551,0.264612821304931,0.206540975098488));
#5894=CARTESIAN_POINT('Ctrl Pts',(1.15809147022147,0.255787504332734,0.213351934557227));
#5895=CARTESIAN_POINT('Ctrl Pts',(1.11706033563968,0.24472949208419,0.220191916744402));
#5896=CARTESIAN_POINT('Ctrl Pts',(1.09724086630217,0.241935102766417,0.220893276198431));
#5897=CARTESIAN_POINT('Ctrl Pts',(1.05683477389847,0.242068991386358,0.216703862540943));
#5898=CARTESIAN_POINT('Ctrl Pts',(1.03718465931368,0.245158125533072,0.211762979306542));
#5899=CARTESIAN_POINT('Ctrl Pts',(0.997159417898573,0.258117110209497,0.195877882014933));
#5900=CARTESIAN_POINT('Ctrl Pts',(0.97827589203717,0.268799087403244,0.184408191234792));
#5901=CARTESIAN_POINT('Ctrl Pts',(0.938511832204562,0.301449132027476,0.1524716629431));
#5902=CARTESIAN_POINT('Ctrl Pts',(0.921897120244161,0.325597462144779,0.130991175878744));
#5903=CARTESIAN_POINT('Ctrl Pts',(0.910735790157152,0.35,0.112156403618172));
#5904=CARTESIAN_POINT('',(1.27550420984285,0.35,-0.132658480043447));
#5905=CARTESIAN_POINT('Origin',(1.1,0.35,0.));
#5906=CARTESIAN_POINT('',(0.910735790157152,0.35,-0.112156403618172));
#5907=CARTESIAN_POINT('Ctrl Pts',(0.910735790157152,0.35,-0.112156403618172));
#5908=CARTESIAN_POINT('Ctrl Pts',(0.917376089752458,0.335482002504965,-0.123361925688084));
#5909=CARTESIAN_POINT('Ctrl Pts',(0.925676503375737,0.321654073155954,-0.135044303040797));
#5910=CARTESIAN_POINT('Ctrl Pts',(0.945705763566752,0.296402587659025,-0.157548233557298));
#5911=CARTESIAN_POINT('Ctrl Pts',(0.957575956315956,0.284823988089694,-0.168539952403236));
#5912=CARTESIAN_POINT('Ctrl Pts',(0.986343324120607,0.264264067609,-0.189265250815529));
#5913=CARTESIAN_POINT('Ctrl Pts',(1.00343254919411,0.255672471019212,-0.198729556237649));
#5914=CARTESIAN_POINT('Ctrl Pts',(1.04053658704398,0.24454764112274,-0.212677811623889));
#5915=CARTESIAN_POINT('Ctrl Pts',(1.05964780090184,0.241866044436253,-0.217181471497843));
#5916=CARTESIAN_POINT('Ctrl Pts',(1.1007627783985,0.242154653351498,-0.221036398352684));
#5917=CARTESIAN_POINT('Ctrl Pts',(1.12185832284616,0.24554830260434,-0.219874810080965));
#5918=CARTESIAN_POINT('Ctrl Pts',(1.16708666484378,0.258980602991006,-0.211069922924208));
#5919=CARTESIAN_POINT('Ctrl Pts',(1.18992721371268,0.270160239182283,-0.202098025620398));
#5920=CARTESIAN_POINT('Ctrl Pts',(1.23829403807689,0.302739787597863,-0.17421352400312));
#5921=CARTESIAN_POINT('Ctrl Pts',(1.2600586328202,0.32583616303801,-0.153092633895047));
#5922=CARTESIAN_POINT('Ctrl Pts',(1.27550420984285,0.35,-0.132658480043447));
#5923=CARTESIAN_POINT('Origin',(1.1,0.35,0.));
#5924=CARTESIAN_POINT('Origin',(-0.339918693812442,0.,1.04616216792467));
#5925=CARTESIAN_POINT('',(-0.559918693812442,0.,1.04616216792467));
#5926=CARTESIAN_POINT('Origin',(-0.339918693812442,0.,1.04616216792467));
#5927=CARTESIAN_POINT('',(-0.559918693812442,0.260874438760115,1.04616216792418));
#5928=CARTESIAN_POINT('',(-0.559918693812442,0.,1.04616216792467));
#5929=CARTESIAN_POINT('',(-0.52031818912536,0.35,1.17208286555157));
#5930=CARTESIAN_POINT('Ctrl Pts',(-0.52031818912536,0.35,1.17208286555157));
#5931=CARTESIAN_POINT('Ctrl Pts',(-0.529217457694123,0.335332571878444,
1.15933338442007));
#5932=CARTESIAN_POINT('Ctrl Pts',(-0.537396458457103,0.321517770338583,
1.14467059284705));
#5933=CARTESIAN_POINT('Ctrl Pts',(-0.550248212225112,0.296532793702566,
1.11286085586034));
#5934=CARTESIAN_POINT('Ctrl Pts',(-0.555078018641098,0.285216775966753,
1.09565550010774));
#5935=CARTESIAN_POINT('Ctrl Pts',(-0.559145317472554,0.270067412950761,
1.06722515592215));
#5936=CARTESIAN_POINT('Ctrl Pts',(-0.559918693812443,0.265170116534296,
1.05680550414918));
#5937=CARTESIAN_POINT('Ctrl Pts',(-0.559918693812443,0.260874438760115,
1.0461621679237));
#5938=CARTESIAN_POINT('',(-0.267986765351098,0.35,1.25407031511432));
#5939=CARTESIAN_POINT('Origin',(-0.339918693812442,0.35,1.04616216792467));
#5940=CARTESIAN_POINT('',(-0.174765758038764,0.35,0.900819442598166));
#5941=CARTESIAN_POINT('Ctrl Pts',(-0.174765758038764,0.35,0.900819442598166));
#5942=CARTESIAN_POINT('Ctrl Pts',(-0.16615910126156,0.335479408675346,0.910599186515575));
#5943=CARTESIAN_POINT('Ctrl Pts',(-0.157611943697822,0.321649098925924,
0.922105787154341));
#5944=CARTESIAN_POINT('Ctrl Pts',(-0.142410854924046,0.296417377297428,
0.948090475176036));
#5945=CARTESIAN_POINT('Ctrl Pts',(-0.135635598256597,0.284856881183445,
0.962749516762522));
#5946=CARTESIAN_POINT('Ctrl Pts',(-0.124807600924643,0.26429242669275,0.996493855518018));
#5947=CARTESIAN_POINT('Ctrl Pts',(-0.12107905659851,0.255687624123886,1.01568738120414));
#5948=CARTESIAN_POINT('Ctrl Pts',(-0.11927397960075,0.244553314150373,1.05530113820794));
#5949=CARTESIAN_POINT('Ctrl Pts',(-0.120893383895271,0.241869161316321,
1.07486553219761));
#5950=CARTESIAN_POINT('Ctrl Pts',(-0.129925208402574,0.242150819014083,
1.11515786183808));
#5951=CARTESIAN_POINT('Ctrl Pts',(-0.137545730009388,0.245541115579871,
1.13486353269143));
#5952=CARTESIAN_POINT('Ctrl Pts',(-0.159894075495139,0.25896926022056,1.17516872094799));
#5953=CARTESIAN_POINT('Ctrl Pts',(-0.175488151194729,0.270150443771654,
1.19412647612185));
#5954=CARTESIAN_POINT('Ctrl Pts',(-0.216960528286492,0.30273418323525,1.2315190249125));
#5955=CARTESIAN_POINT('Ctrl Pts',(-0.243776713476772,0.325833097600423,
1.24569413677302));
#5956=CARTESIAN_POINT('Ctrl Pts',(-0.267986765351098,0.35,1.25407031511432));
#5957=CARTESIAN_POINT('',(-0.388099915049348,0.35,0.831502973106184));
#5958=CARTESIAN_POINT('Origin',(-0.339918693812442,0.35,1.04616216792467));
#5959=CARTESIAN_POINT('Ctrl Pts',(-0.559918693812442,0.260874438760115,
1.0461621679237));
#5960=CARTESIAN_POINT('Ctrl Pts',(-0.559918693812441,0.256572067929757,
1.03550224841356));
#5961=CARTESIAN_POINT('Ctrl Pts',(-0.55914412823418,0.252872176837747,1.02461835660205));
#5962=CARTESIAN_POINT('Ctrl Pts',(-0.554627960771623,0.244745328150166,
0.994433608378459));
#5963=CARTESIAN_POINT('Ctrl Pts',(-0.549175023311743,0.241941375180247,
0.975354466173215));
#5964=CARTESIAN_POINT('Ctrl Pts',(-0.532711855060331,0.242062069598183,
0.938206075044726));
#5965=CARTESIAN_POINT('Ctrl Pts',(-0.521946739366383,0.245143826724662,
0.921041750757786));
#5966=CARTESIAN_POINT('Ctrl Pts',(-0.494476822014916,0.25808943656053,0.887869891643464));
#5967=CARTESIAN_POINT('Ctrl Pts',(-0.477731860324512,0.268767859044401,
0.873445791067852));
#5968=CARTESIAN_POINT('Ctrl Pts',(-0.435054453498551,0.301421636034264,
0.84547220309525));
#5969=CARTESIAN_POINT('Ctrl Pts',(-0.409474560891576,0.325582986157859,
0.836300608451158));
#5970=CARTESIAN_POINT('Ctrl Pts',(-0.388099915049348,0.35,0.831502973106184));
#5971=CARTESIAN_POINT('Origin',(0.889918693812442,0.,0.64656377752172));
#5972=CARTESIAN_POINT('',(0.669918693812442,0.,0.64656377752172));
#5973=CARTESIAN_POINT('Origin',(0.889918693812442,0.,0.64656377752172));
#5974=CARTESIAN_POINT('',(0.669918693812442,0.328688122539757,0.646563777561565));
#5975=CARTESIAN_POINT('',(0.669918693812442,0.,0.64656377752172));
#5976=CARTESIAN_POINT('',(0.953929883998579,0.35,0.857045528585688));
#5977=CARTESIAN_POINT('Ctrl Pts',(0.953929883998579,0.35,0.857045528585689));
#5978=CARTESIAN_POINT('Ctrl Pts',(0.939113614143973,0.335390975831827,0.861551415973636));
#5979=CARTESIAN_POINT('Ctrl Pts',(0.922713318211476,0.32162844535795,0.864791301338213));
#5980=CARTESIAN_POINT('Ctrl Pts',(0.888689691679126,0.296761201350329,0.867202773669637));
#5981=CARTESIAN_POINT('Ctrl Pts',(0.87096870334968,0.285505993520706,0.866515344265356));
#5982=CARTESIAN_POINT('Ctrl Pts',(0.832657955828335,0.264913063744833,0.859966994580058));
#5983=CARTESIAN_POINT('Ctrl Pts',(0.812042610895507,0.255983013500831,0.853529132681505));
#5984=CARTESIAN_POINT('Ctrl Pts',(0.774637004578398,0.244799211872409,0.834944631013122));
#5985=CARTESIAN_POINT('Ctrl Pts',(0.758129671802899,0.241962745238242,0.823863745365518));
#5986=CARTESIAN_POINT('Ctrl Pts',(0.72783201892456,0.242038904448235,0.796734896229851));
#5987=CARTESIAN_POINT('Ctrl Pts',(0.714819045120535,0.245095813663096,0.781209421868765));
#5988=CARTESIAN_POINT('Ctrl Pts',(0.691707150272297,0.257996207173293,0.744838566725142));
#5989=CARTESIAN_POINT('Ctrl Pts',(0.683135660593065,0.268662345405231,0.724442597621042));
#5990=CARTESIAN_POINT('Ctrl Pts',(0.672013600394921,0.29561651331323,0.683754327616304));
#5991=CARTESIAN_POINT('Ctrl Pts',(0.669918693818778,0.311769951237127,0.664055407862726));
#5992=CARTESIAN_POINT('Ctrl Pts',(0.669918693812442,0.328688122539757,0.646563777601409));
#5993=CARTESIAN_POINT('',(1.10987928032073,0.35,0.642399598979491));
#5994=CARTESIAN_POINT('Origin',(0.889918693812442,0.35,0.64656377752172));
#5995=CARTESIAN_POINT('',(0.802724611619556,0.35,0.444580629634229));
#5996=CARTESIAN_POINT('Ctrl Pts',(0.802724611619556,0.35,0.444580629634229));
#5997=CARTESIAN_POINT('Ctrl Pts',(0.814693298418458,0.335469703254327,0.439413868588077));
#5998=CARTESIAN_POINT('Ctrl Pts',(0.828288194978147,0.321630486900879,0.434838103866291));
#5999=CARTESIAN_POINT('Ctrl Pts',(0.857626293279467,0.296466623645907,0.428430764212231));
#6000=CARTESIAN_POINT('Ctrl Pts',(0.873562500583475,0.284968850954313,0.426522755127025));
#6001=CARTESIAN_POINT('Ctrl Pts',(0.908944175205009,0.264389371081103,0.426610046318699));
#6002=CARTESIAN_POINT('Ctrl Pts',(0.928411894256451,0.255739222721824,0.428985062409479));
#6003=CARTESIAN_POINT('Ctrl Pts',(0.966701070362238,0.244572490203357,0.439509162402782));
#6004=CARTESIAN_POINT('Ctrl Pts',(0.984800606765884,0.24187970665778,0.447081989738821));
#6005=CARTESIAN_POINT('Ctrl Pts',(1.02033222655978,0.242137933247099,0.468098181585364));
#6006=CARTESIAN_POINT('Ctrl Pts',(1.03672671564999,0.245516880218307,0.48142671327546));
#6007=CARTESIAN_POINT('Ctrl Pts',(1.0681914718434,0.258930838869849,0.515141616697554));
#6008=CARTESIAN_POINT('Ctrl Pts',(1.08142350523446,0.270117119131827,0.535848665318464));
#6009=CARTESIAN_POINT('Ctrl Pts',(1.10419503710793,0.302714929726697,0.586877157140452));
#6010=CARTESIAN_POINT('Ctrl Pts',(1.10939416747485,0.325822565838313,0.616774927746317));
#6011=CARTESIAN_POINT('Ctrl Pts',(1.10987928032073,0.35,0.642399598979492));
#6012=CARTESIAN_POINT('',(0.670876851625708,0.35,0.626053502744384));
#6013=CARTESIAN_POINT('Origin',(0.889918693812442,0.35,0.64656377752172));
#6014=CARTESIAN_POINT('Ctrl Pts',(0.669918693812442,0.328688122539757,0.646563777601409));
#6015=CARTESIAN_POINT('Ctrl Pts',(0.669918693809818,0.335695203413973,0.639319184455347));
#6016=CARTESIAN_POINT('Ctrl Pts',(0.670277510265801,0.342834510102275,0.632454237839257));
#6017=CARTESIAN_POINT('Ctrl Pts',(0.670876851625708,0.35,0.626053502744384));
#6018=CARTESIAN_POINT('Origin',(0.339918693812442,0.,1.04616216792467));
#6019=CARTESIAN_POINT('',(0.119918693812442,0.,1.04616216792467));
#6020=CARTESIAN_POINT('Origin',(0.339918693812442,0.,1.04616216792467));
#6021=CARTESIAN_POINT('',(0.119918693812442,0.247376716776579,1.04616216792467));
#6022=CARTESIAN_POINT('',(0.119918693812442,0.,1.04616216792467));
#6023=CARTESIAN_POINT('',(0.267986765351098,0.35,1.25407031511432));
#6024=CARTESIAN_POINT('Ctrl Pts',(0.267986765351098,0.35,1.25407031511432));
#6025=CARTESIAN_POINT('Ctrl Pts',(0.253293148857988,0.335332571878444,1.24898662703038));
#6026=CARTESIAN_POINT('Ctrl Pts',(0.238057625599671,0.321517770338583,1.2419316754898));
#6027=CARTESIAN_POINT('Ctrl Pts',(0.20896304411374,0.296532793702567,1.22375112901188));
#6028=CARTESIAN_POINT('Ctrl Pts',(0.194942594271844,0.285216775966753,1.21267059279651));
#6029=CARTESIAN_POINT('Ctrl Pts',(0.16782911650589,0.264680669899338,1.18473227113195));
#6030=CARTESIAN_POINT('Ctrl Pts',(0.155029153917439,0.255831783241443,1.16745023332297));
#6031=CARTESIAN_POINT('Ctrl Pts',(0.135809963569083,0.244745328150166,1.13051582480638));
#6032=CARTESIAN_POINT('Ctrl Pts',(0.129007044228756,0.241941375180247,1.11187531830365));
#6033=CARTESIAN_POINT('Ctrl Pts',(0.121501840920506,0.242047740248445,1.07686180187776));
#6034=CARTESIAN_POINT('Ctrl Pts',(0.119918693812442,0.243865919483247,1.06140091782046));
#6035=CARTESIAN_POINT('Ctrl Pts',(0.119918693812442,0.247376716776579,1.04616216792467));
#6036=CARTESIAN_POINT('',(0.52031818912536,0.35,1.17208286555157));
#6037=CARTESIAN_POINT('Origin',(0.339918693812442,0.35,1.04616216792467));
#6038=CARTESIAN_POINT('',(0.388099915049348,0.35,0.831502973106184));
#6039=CARTESIAN_POINT('Ctrl Pts',(0.388099915049349,0.35,0.831502973106184));
#6040=CARTESIAN_POINT('Ctrl Pts',(0.400811235892708,0.335479408675346,0.83435608621082));
#6041=CARTESIAN_POINT('Ctrl Pts',(0.414489441774859,0.321649098925924,0.838641228510082));
#6042=CARTESIAN_POINT('Ctrl Pts',(0.442060797330419,0.296417377297427,0.85072830691315));
#6043=CARTESIAN_POINT('Ctrl Pts',(0.456158463572915,0.284856881183445,0.858605324728243));
#6044=CARTESIAN_POINT('Ctrl Pts',(0.484752922098352,0.264292426692752,0.879540531101798));
#6045=CARTESIAN_POINT('Ctrl Pts',(0.499051049160275,0.255687624123886,0.892876836196423));
#6046=CARTESIAN_POINT('Ctrl Pts',(0.523795769282349,0.244553314150373,0.923864041185));
#6047=CARTESIAN_POINT('Ctrl Pts',(0.533985305944486,0.241869161316321,0.940643830369109));
#6048=CARTESIAN_POINT('Ctrl Pts',(0.550361643571045,0.242150819014083,0.9785497830379));
#6049=CARTESIAN_POINT('Ctrl Pts',(0.555779214799254,0.245541115579872,0.998971235859074));
#6050=CARTESIAN_POINT('Ctrl Pts',(0.561389818753198,0.25896926022056,1.04471484600977));
#6051=CARTESIAN_POINT('Ctrl Pts',(0.559917035408429,0.270150443771653,1.06921795983998));
#6052=CARTESIAN_POINT('Ctrl Pts',(0.548343966268834,0.30273418323525,1.12384601890666));
#6053=CARTESIAN_POINT('Ctrl Pts',(0.534981138426803,0.325833097600422,1.15107608347657));
#6054=CARTESIAN_POINT('Ctrl Pts',(0.52031818912536,0.35,1.17208286555157));
#6055=CARTESIAN_POINT('',(0.174765758038764,0.35,0.900819442598166));
#6056=CARTESIAN_POINT('Origin',(0.339918693812442,0.35,1.04616216792467));
#6057=CARTESIAN_POINT('Ctrl Pts',(0.119918693812442,0.247376716776579,1.04616216792467));
#6058=CARTESIAN_POINT('Ctrl Pts',(0.119918693812442,0.248451342886481,1.04149771220363));
#6059=CARTESIAN_POINT('Ctrl Pts',(0.120067055145306,0.249684690290744,1.03685410010078));
#6060=CARTESIAN_POINT('Ctrl Pts',(0.121836675927961,0.25808943656053,1.00894801471422));
#6061=CARTESIAN_POINT('Ctrl Pts',(0.126905360909727,0.268767859044402,0.987436230688157));
#6062=CARTESIAN_POINT('Ctrl Pts',(0.144989645843781,0.301421636034262,0.939719972286297));
#6063=CARTESIAN_POINT('Ctrl Pts',(0.160293285605306,0.325582986157856,0.917264512724103));
#6064=CARTESIAN_POINT('Ctrl Pts',(0.174765758038763,0.35,0.900819442598166));
#6065=CARTESIAN_POINT('Origin',(-0.889918693812442,0.,0.646563777521721));
#6066=CARTESIAN_POINT('',(-1.10991869381244,0.,0.646563777521721));
#6067=CARTESIAN_POINT('Origin',(-0.889918693812442,0.,0.646563777521721));
#6068=CARTESIAN_POINT('',(-1.10991869381244,0.35,0.646563777521721));
#6069=CARTESIAN_POINT('',(-1.10991869381244,0.,0.646563777521721));
#6070=CARTESIAN_POINT('',(-0.953929883998579,0.35,0.857045528585689));
#6071=CARTESIAN_POINT('Origin',(-0.889918693812442,0.35,0.646563777521721));
#6072=CARTESIAN_POINT('',(-0.670876851625708,0.35,0.626053502744384));
#6073=CARTESIAN_POINT('Ctrl Pts',(-0.670876851625708,0.35,0.626053502744384));
#6074=CARTESIAN_POINT('Ctrl Pts',(-0.669661497485836,0.335469703254326,
0.639033017285111));
#6075=CARTESIAN_POINT('Ctrl Pts',(-0.669510740703862,0.321630486900879,
0.653376521307855));
#6076=CARTESIAN_POINT('Ctrl Pts',(-0.672482969531502,0.296466623645907,
0.68325868771487));
#6077=CARTESIAN_POINT('Ctrl Pts',(-0.675592903940688,0.284968850954313,
0.699004528749127));
#6078=CARTESIAN_POINT('Ctrl Pts',(-0.686609461544843,0.264389371081103,
0.732627526493686));
#6079=CARTESIAN_POINT('Ctrl Pts',(-0.694884092102898,0.255739222721824,
0.750408507220998));
#6080=CARTESIAN_POINT('Ctrl Pts',(-0.716725112096974,0.244572490203356,
0.783571551911549));
#6081=CARTESIAN_POINT('Ctrl Pts',(-0.729520363220728,0.24187970665778,0.798445101607853));
#6082=CARTESIAN_POINT('Ctrl Pts',(-0.760487823778074,0.242137933247099,
0.825743319709735));
#6083=CARTESIAN_POINT('Ctrl Pts',(-0.778230186437554,0.245516880218307,
0.837216662588005));
#6084=CARTESIAN_POINT('Ctrl Pts',(-0.820018109421027,0.258930838869848,
0.856722945878246));
#6085=CARTESIAN_POINT('Ctrl Pts',(-0.843800606133157,0.270117119131826,
0.862908527531438));
#6086=CARTESIAN_POINT('Ctrl Pts',(-0.899368376134038,0.302714929726702,
0.868796870135415));
#6087=CARTESIAN_POINT('Ctrl Pts',(-0.929409465330792,0.325822565838321,
0.864502617738802));
#6088=CARTESIAN_POINT('Ctrl Pts',(-0.95392988399858,0.35,0.857045528585688));
#6089=CARTESIAN_POINT('',(-0.802724611619556,0.35,0.444580629634229));
#6090=CARTESIAN_POINT('Origin',(-0.889918693812442,0.35,0.646563777521721));
#6091=CARTESIAN_POINT('',(-1.10987928032073,0.35,0.642399598979491));
#6092=CARTESIAN_POINT('Ctrl Pts',(-1.10987928032073,0.35,0.642399598979492));
#6093=CARTESIAN_POINT('Ctrl Pts',(-1.10958615470441,0.335390975831827,0.626916093209464));
#6094=CARTESIAN_POINT('Ctrl Pts',(-1.10759949863652,0.321628445357949,0.610317305256213));
#6095=CARTESIAN_POINT('Ctrl Pts',(-1.09937906630242,0.296761201350329,0.577213727602755));
#6096=CARTESIAN_POINT('Ctrl Pts',(-1.09324919553707,0.285505993520706,0.5605724935452));
#6097=CARTESIAN_POINT('Ctrl Pts',(-1.07518267284658,0.264913063744833,0.526160358808755));
#6098=CARTESIAN_POINT('Ctrl Pts',(-1.06268941040781,0.255983013500831,0.508543409408808));
#6099=CARTESIAN_POINT('Ctrl Pts',(-1.03345553095711,0.244799211872409,0.478711490622469));
#6100=CARTESIAN_POINT('Ctrl Pts',(-1.0178159360962,0.241962745238242,0.466436266197514));
#6101=CARTESIAN_POINT('Ctrl Pts',(-0.982652377717061,0.242038904448235,
0.446004761419877));
#6102=CARTESIAN_POINT('Ctrl Pts',(-0.963865544104578,0.245095813663095,
0.438426323310488));
#6103=CARTESIAN_POINT('Ctrl Pts',(-0.922132837036694,0.257996207173294,
0.427684817450471));
#6104=CARTESIAN_POINT('Ctrl Pts',(-0.900086381736091,0.268662345405233,
0.425835547406596));
#6105=CARTESIAN_POINT('Ctrl Pts',(-0.849024073352861,0.301328368152829,
0.428254106385369));
#6106=CARTESIAN_POINT('Ctrl Pts',(-0.822877500049854,0.325533869830937,
0.435880831514466));
#6107=CARTESIAN_POINT('Ctrl Pts',(-0.802724611619556,0.35,0.444580629634229));
#6108=CARTESIAN_POINT('Origin',(-0.889918693812442,0.35,0.646563777521721));
#6109=CARTESIAN_POINT('Origin',(-1.1,0.,1.34711147906209E-16));
#6110=CARTESIAN_POINT('',(-1.32,0.,1.61653377487451E-16));
#6111=CARTESIAN_POINT('Origin',(-1.1,0.,1.34711147906209E-16));
#6112=CARTESIAN_POINT('',(-1.32,0.35,1.61653377487451E-16));
#6113=CARTESIAN_POINT('',(-1.32,0.,1.61653377487451E-16));
#6114=CARTESIAN_POINT('',(-1.27550420984285,0.35,0.132658480043447));
#6115=CARTESIAN_POINT('Origin',(-1.1,0.35,1.34711147906209E-16));
#6116=CARTESIAN_POINT('',(-0.910735790157152,0.35,0.112156403618172));
#6117=CARTESIAN_POINT('Ctrl Pts',(-0.910735790157152,0.35,0.112156403618173));
#6118=CARTESIAN_POINT('Ctrl Pts',(-0.917376089752458,0.335482002504965,
0.123361925688084));
#6119=CARTESIAN_POINT('Ctrl Pts',(-0.925676503375737,0.321654073155954,
0.135044303040797));
#6120=CARTESIAN_POINT('Ctrl Pts',(-0.945705763566752,0.296402587659025,
0.157548233557298));
#6121=CARTESIAN_POINT('Ctrl Pts',(-0.957575956315956,0.284823988089694,
0.168539952403237));
#6122=CARTESIAN_POINT('Ctrl Pts',(-0.986343324120607,0.264264067609,0.189265250815529));
#6123=CARTESIAN_POINT('Ctrl Pts',(-1.00343254919411,0.255672471019212,0.198729556237649));
#6124=CARTESIAN_POINT('Ctrl Pts',(-1.04053658704398,0.24454764112274,0.21267781162389));
#6125=CARTESIAN_POINT('Ctrl Pts',(-1.05964780090184,0.241866044436253,0.217181471497844));
#6126=CARTESIAN_POINT('Ctrl Pts',(-1.1007627783985,0.242154653351498,0.221036398352684));
#6127=CARTESIAN_POINT('Ctrl Pts',(-1.12185832284616,0.24554830260434,0.219874810080966));
#6128=CARTESIAN_POINT('Ctrl Pts',(-1.16708666484378,0.258980602991006,0.211069922924208));
#6129=CARTESIAN_POINT('Ctrl Pts',(-1.18992721371268,0.270160239182283,0.202098025620397));
#6130=CARTESIAN_POINT('Ctrl Pts',(-1.23829403807689,0.302739787597863,0.174213524003119));
#6131=CARTESIAN_POINT('Ctrl Pts',(-1.2600586328202,0.325836163038011,0.153092633895046));
#6132=CARTESIAN_POINT('Ctrl Pts',(-1.27550420984285,0.35,0.132658480043447));
#6133=CARTESIAN_POINT('',(-0.910735790157152,0.35,-0.112156403618172));
#6134=CARTESIAN_POINT('Origin',(-1.1,0.35,1.34711147906209E-16));
#6135=CARTESIAN_POINT('',(-1.27550420984285,0.35,-0.132658480043447));
#6136=CARTESIAN_POINT('Ctrl Pts',(-1.27550420984285,0.35,-0.132658480043447));
#6137=CARTESIAN_POINT('Ctrl Pts',(-1.26611782177473,0.335315462762739,-0.145076462072449));
#6138=CARTESIAN_POINT('Ctrl Pts',(-1.25468431627751,0.321485352158938,-0.157400492027332));
#6139=CARTESIAN_POINT('Ctrl Pts',(-1.22835219222699,0.296466041103173,-0.179483010322184));
#6140=CARTESIAN_POINT('Ctrl Pts',(-1.21344338101808,0.285132356747975,-0.189407731207313));
#6141=CARTESIAN_POINT('Ctrl Pts',(-1.17846267135551,0.264612821304931,-0.206540975098488));
#6142=CARTESIAN_POINT('Ctrl Pts',(-1.15809147022147,0.255787504332734,-0.213351934557227));
#6143=CARTESIAN_POINT('Ctrl Pts',(-1.11706033563968,0.24472949208419,-0.220191916744402));
#6144=CARTESIAN_POINT('Ctrl Pts',(-1.09724086630217,0.241935102766417,-0.22089327619843));
#6145=CARTESIAN_POINT('Ctrl Pts',(-1.05683477389847,0.242068991386358,-0.216703862540943));
#6146=CARTESIAN_POINT('Ctrl Pts',(-1.03718465931368,0.245158125533072,-0.211762979306542));
#6147=CARTESIAN_POINT('Ctrl Pts',(-0.997159417898573,0.258117110209497,
-0.195877882014933));
#6148=CARTESIAN_POINT('Ctrl Pts',(-0.978275892037171,0.268799087403243,
-0.184408191234793));
#6149=CARTESIAN_POINT('Ctrl Pts',(-0.938511832204561,0.301449132027478,
-0.152471662943099));
#6150=CARTESIAN_POINT('Ctrl Pts',(-0.92189712024416,0.325597462144781,-0.130991175878742));
#6151=CARTESIAN_POINT('Ctrl Pts',(-0.910735790157152,0.35,-0.112156403618172));
#6152=CARTESIAN_POINT('Origin',(-1.1,0.35,1.34711147906209E-16));
#6153=CARTESIAN_POINT('Origin',(-0.339918693812442,0.,-1.04616216792467));
#6154=CARTESIAN_POINT('',(-0.559918693812442,0.,-1.04616216792467));
#6155=CARTESIAN_POINT('Origin',(-0.339918693812442,0.,-1.04616216792467));
#6156=CARTESIAN_POINT('',(-0.559918693812442,0.26087443875944,-1.04616216792335));
#6157=CARTESIAN_POINT('',(-0.559918693812442,0.,-1.04616216792467));
#6158=CARTESIAN_POINT('',(-0.388099915049348,0.35,-0.831502973106184));
#6159=CARTESIAN_POINT('Ctrl Pts',(-0.388099915049349,0.35,-0.831502973106184));
#6160=CARTESIAN_POINT('Ctrl Pts',(-0.400811235892708,0.335479408675346,
-0.83435608621082));
#6161=CARTESIAN_POINT('Ctrl Pts',(-0.414489441774859,0.321649098925924,
-0.838641228510082));
#6162=CARTESIAN_POINT('Ctrl Pts',(-0.442060797330419,0.296417377297428,
-0.85072830691315));
#6163=CARTESIAN_POINT('Ctrl Pts',(-0.456158463572915,0.284856881183445,
-0.858605324728243));
#6164=CARTESIAN_POINT('Ctrl Pts',(-0.484752922098354,0.264292426692751,
-0.879540531101799));
#6165=CARTESIAN_POINT('Ctrl Pts',(-0.499051049160275,0.255687624123886,
-0.892876836196423));
#6166=CARTESIAN_POINT('Ctrl Pts',(-0.523795769282349,0.244553314150373,
-0.923864041185001));
#6167=CARTESIAN_POINT('Ctrl Pts',(-0.533985305944486,0.241869161316321,
-0.94064383036911));
#6168=CARTESIAN_POINT('Ctrl Pts',(-0.550361643571044,0.242150819014083,
-0.9785497830379));
#6169=CARTESIAN_POINT('Ctrl Pts',(-0.555779214799254,0.245541115579872,
-0.998971235859074));
#6170=CARTESIAN_POINT('Ctrl Pts',(-0.559392545156815,0.254189083441125,
-1.02843094760825));
#6171=CARTESIAN_POINT('Ctrl Pts',(-0.559918693812337,0.257327896059345,
-1.03737495240447));
#6172=CARTESIAN_POINT('Ctrl Pts',(-0.559918693812442,0.26087443875944,-1.04616216792202));
#6173=CARTESIAN_POINT('',(-0.174765758038764,0.35,-0.900819442598166));
#6174=CARTESIAN_POINT('Origin',(-0.339918693812442,0.35,-1.04616216792467));
#6175=CARTESIAN_POINT('',(-0.267986765351098,0.35,-1.25407031511432));
#6176=CARTESIAN_POINT('Ctrl Pts',(-0.267986765351098,0.35,-1.25407031511432));
#6177=CARTESIAN_POINT('Ctrl Pts',(-0.253293148857987,0.335332571878443,
-1.24898662703038));
#6178=CARTESIAN_POINT('Ctrl Pts',(-0.23805762559967,0.321517770338583,-1.2419316754898));
#6179=CARTESIAN_POINT('Ctrl Pts',(-0.208963044113739,0.296532793702567,
-1.22375112901188));
#6180=CARTESIAN_POINT('Ctrl Pts',(-0.194942594271844,0.285216775966753,
-1.21267059279651));
#6181=CARTESIAN_POINT('Ctrl Pts',(-0.167829116505892,0.264680669899339,
-1.18473227113195));
#6182=CARTESIAN_POINT('Ctrl Pts',(-0.155029153917439,0.255831783241444,
-1.16745023332297));
#6183=CARTESIAN_POINT('Ctrl Pts',(-0.135809963569083,0.244745328150166,
-1.13051582480638));
#6184=CARTESIAN_POINT('Ctrl Pts',(-0.129007044228756,0.241941375180247,
-1.11187531830365));
#6185=CARTESIAN_POINT('Ctrl Pts',(-0.120490750673684,0.242062069598183,
-1.07214483106283));
#6186=CARTESIAN_POINT('Ctrl Pts',(-0.119110975535071,0.245143826724661,
-1.05193102477361));
#6187=CARTESIAN_POINT('Ctrl Pts',(-0.121836675927961,0.25808943656053,-1.00894801471422));
#6188=CARTESIAN_POINT('Ctrl Pts',(-0.126905360909727,0.268767859044401,
-0.987436230688157));
#6189=CARTESIAN_POINT('Ctrl Pts',(-0.144989645843782,0.301421636034265,
-0.939719972286292));
#6190=CARTESIAN_POINT('Ctrl Pts',(-0.160293285605309,0.325582986157861,
-0.9172645127241));
#6191=CARTESIAN_POINT('Ctrl Pts',(-0.174765758038764,0.35,-0.900819442598166));
#6192=CARTESIAN_POINT('',(-0.52031818912536,0.35,-1.17208286555157));
#6193=CARTESIAN_POINT('Origin',(-0.339918693812442,0.35,-1.04616216792467));
#6194=CARTESIAN_POINT('Ctrl Pts',(-0.559918693812442,0.26087443875944,-1.04616216792202));
#6195=CARTESIAN_POINT('Ctrl Pts',(-0.559918693812632,0.267254559470881,
-1.0619700970689));
#6196=CARTESIAN_POINT('Ctrl Pts',(-0.558211019996387,0.274953695271867,
-1.07727082028465));
#6197=CARTESIAN_POINT('Ctrl Pts',(-0.548343966268835,0.302734183235248,
-1.12384601890665));
#6198=CARTESIAN_POINT('Ctrl Pts',(-0.534981138426805,0.325833097600418,
-1.15107608347657));
#6199=CARTESIAN_POINT('Ctrl Pts',(-0.52031818912536,0.35,-1.17208286555157));
#6200=CARTESIAN_POINT('Origin',(0.889918693812442,0.,-0.646563777521721));
#6201=CARTESIAN_POINT('',(0.669918693812442,0.,-0.646563777521721));
#6202=CARTESIAN_POINT('Origin',(0.889918693812442,0.,-0.646563777521721));
#6203=CARTESIAN_POINT('',(0.669918693812442,0.328688122609646,-0.646563777525436));
#6204=CARTESIAN_POINT('',(0.669918693812442,0.,-0.646563777521721));
#6205=CARTESIAN_POINT('',(0.670876851625708,0.35,-0.626053502744384));
#6206=CARTESIAN_POINT('Ctrl Pts',(0.670876851625708,0.35,-0.626053502744384));
#6207=CARTESIAN_POINT('Ctrl Pts',(0.670266054477489,0.34269754919667,-0.632576581250196));
#6208=CARTESIAN_POINT('Ctrl Pts',(0.669918693812202,0.335572060345374,-0.639446501589323));
#6209=CARTESIAN_POINT('Ctrl Pts',(0.669918693812442,0.328688122609646,-0.646563777529151));
#6210=CARTESIAN_POINT('',(0.802724611619556,0.35,-0.444580629634229));
#6211=CARTESIAN_POINT('Origin',(0.889918693812442,0.35,-0.646563777521721));
#6212=CARTESIAN_POINT('',(1.10987928032073,0.35,-0.642399598979491));
#6213=CARTESIAN_POINT('Ctrl Pts',(1.10987928032073,0.35,-0.642399598979492));
#6214=CARTESIAN_POINT('Ctrl Pts',(1.10958615470441,0.335390975831828,-0.626916093209466));
#6215=CARTESIAN_POINT('Ctrl Pts',(1.10759949863652,0.32162844535795,-0.610317305256214));
#6216=CARTESIAN_POINT('Ctrl Pts',(1.09937906630242,0.296761201350329,-0.577213727602755));
#6217=CARTESIAN_POINT('Ctrl Pts',(1.09324919553707,0.285505993520706,-0.560572493545201));
#6218=CARTESIAN_POINT('Ctrl Pts',(1.07518267284658,0.264913063744833,-0.526160358808756));
#6219=CARTESIAN_POINT('Ctrl Pts',(1.06268941040781,0.255983013500831,-0.508543409408808));
#6220=CARTESIAN_POINT('Ctrl Pts',(1.03345553095711,0.244799211872409,-0.478711490622469));
#6221=CARTESIAN_POINT('Ctrl Pts',(1.0178159360962,0.241962745238242,-0.466436266197514));
#6222=CARTESIAN_POINT('Ctrl Pts',(0.982652377717061,0.242038904448235,-0.446004761419877));
#6223=CARTESIAN_POINT('Ctrl Pts',(0.963865544104578,0.245095813663095,-0.438426323310488));
#6224=CARTESIAN_POINT('Ctrl Pts',(0.922132837036694,0.257996207173294,-0.427684817450471));
#6225=CARTESIAN_POINT('Ctrl Pts',(0.900086381736092,0.268662345405233,-0.425835547406596));
#6226=CARTESIAN_POINT('Ctrl Pts',(0.849024073352859,0.30132836815283,-0.428254106385369));
#6227=CARTESIAN_POINT('Ctrl Pts',(0.822877500049852,0.32553386983094,-0.435880831514467));
#6228=CARTESIAN_POINT('Ctrl Pts',(0.802724611619556,0.35,-0.444580629634229));
#6229=CARTESIAN_POINT('',(0.953929883998579,0.35,-0.857045528585689));
#6230=CARTESIAN_POINT('Origin',(0.889918693812442,0.35,-0.646563777521721));
#6231=CARTESIAN_POINT('Ctrl Pts',(0.669918693812442,0.328688122609646,-0.646563777529151));
#6232=CARTESIAN_POINT('Ctrl Pts',(0.66991869381268,0.32187451403212,-0.65360834043107));
#6233=CARTESIAN_POINT('Ctrl Pts',(0.670258663808197,0.31529832480498,-0.66089598362366));
#6234=CARTESIAN_POINT('Ctrl Pts',(0.672482969531502,0.296466623645907,-0.68325868771487));
#6235=CARTESIAN_POINT('Ctrl Pts',(0.675592903940687,0.284968850954313,-0.699004528749128));
#6236=CARTESIAN_POINT('Ctrl Pts',(0.686609461544843,0.264389371081104,-0.732627526493686));
#6237=CARTESIAN_POINT('Ctrl Pts',(0.694884092102897,0.255739222721825,-0.750408507220998));
#6238=CARTESIAN_POINT('Ctrl Pts',(0.716725112096974,0.244572490203356,-0.783571551911549));
#6239=CARTESIAN_POINT('Ctrl Pts',(0.729520363220727,0.24187970665778,-0.798445101607854));
#6240=CARTESIAN_POINT('Ctrl Pts',(0.760487823778074,0.242137933247099,-0.825743319709736));
#6241=CARTESIAN_POINT('Ctrl Pts',(0.778230186437555,0.245516880218307,-0.837216662588005));
#6242=CARTESIAN_POINT('Ctrl Pts',(0.820018109421027,0.258930838869848,-0.856722945878246));
#6243=CARTESIAN_POINT('Ctrl Pts',(0.843800606133157,0.270117119131827,-0.862908527531438));
#6244=CARTESIAN_POINT('Ctrl Pts',(0.899368376134036,0.302714929726701,-0.868796870135415));
#6245=CARTESIAN_POINT('Ctrl Pts',(0.92940946533079,0.325822565838319,-0.864502617738803));
#6246=CARTESIAN_POINT('Ctrl Pts',(0.953929883998579,0.35,-0.857045528585689));
#6247=CARTESIAN_POINT('Origin',(1.4,0.35,0.));
#6248=CARTESIAN_POINT('Origin',(0.,0.35,0.));
#6249=CARTESIAN_POINT('Origin',(0.,0.35,0.));
#6250=CARTESIAN_POINT('Origin',(0.,0.35,0.));
#6251=CARTESIAN_POINT('Origin',(0.,0.35,0.));
#6252=CARTESIAN_POINT('Origin',(0.,0.35,0.));
#6253=CARTESIAN_POINT('Origin',(0.,0.35,0.));
#6254=CARTESIAN_POINT('Origin',(0.,0.35,0.));
#6255=CARTESIAN_POINT('Origin',(0.,0.35,0.));
#6256=CARTESIAN_POINT('Origin',(0.,0.35,0.));
#6257=CARTESIAN_POINT('Origin',(0.,0.35,0.));
#6258=CARTESIAN_POINT('',(-0.75,0.35,-9.18485099360515E-17));
#6259=CARTESIAN_POINT('Origin',(0.,0.35,0.));
#6260=CARTESIAN_POINT('Origin',(0.,0.45,0.));
#6261=CARTESIAN_POINT('Origin',(0.,0.35,0.));
#6262=CARTESIAN_POINT('Origin',(0.,0.45,0.));
#6263=CARTESIAN_POINT('Origin',(0.,0.35,0.));
#6264=CARTESIAN_POINT('Origin',(0.,0.45,0.));
#6265=CARTESIAN_POINT('Origin',(0.,0.35,0.));
#6266=CARTESIAN_POINT('Origin',(0.,0.45,0.));
#6267=CARTESIAN_POINT('Origin',(0.,0.35,0.));
#6268=CARTESIAN_POINT('Origin',(0.,0.45,0.));
#6269=CARTESIAN_POINT('Origin',(0.,0.35,0.));
#6270=CARTESIAN_POINT('Origin',(0.,0.45,0.));
#6271=CARTESIAN_POINT('Origin',(0.,0.35,0.));
#6272=CARTESIAN_POINT('Origin',(0.,0.45,0.));
#6273=CARTESIAN_POINT('Origin',(0.,0.35,0.));
#6274=CARTESIAN_POINT('Origin',(0.,0.45,0.));
#6275=CARTESIAN_POINT('Origin',(0.,0.35,0.));
#6276=CARTESIAN_POINT('Origin',(0.,0.45,0.));
#6277=CARTESIAN_POINT('Origin',(0.,0.35,0.));
#6278=CARTESIAN_POINT('Origin',(0.,0.45,0.));
#6279=CARTESIAN_POINT('Origin',(0.,0.35,0.));
#6280=CARTESIAN_POINT('Origin',(1.4,0.35,0.));
#6281=CARTESIAN_POINT('',(-1.4,0.35,-1.71450551880629E-16));
#6282=CARTESIAN_POINT('Origin',(0.,0.35,0.));
#6283=CARTESIAN_POINT('Origin',(0.,0.175,0.));
#6284=CARTESIAN_POINT('',(-1.4,0.,-1.71450551880629E-16));
#6285=CARTESIAN_POINT('Origin',(0.,0.,0.));
#6286=CARTESIAN_POINT('',(-1.4,0.175,-1.71450551880629E-16));
#6287=CARTESIAN_POINT('Origin',(0.75,0.,0.));
#6288=CARTESIAN_POINT('',(-0.75,0.,-9.18485099360515E-17));
#6289=CARTESIAN_POINT('Origin',(0.,0.,0.));
#6290=CARTESIAN_POINT('Origin',(0.,0.175,0.));
#6291=CARTESIAN_POINT('',(-0.75,0.175,-9.18485099360515E-17));
#6292=CARTESIAN_POINT('',(0.,0.,0.));
#6293=CARTESIAN_POINT('Origin',(0.339918693812442,0.,-1.04616216792467));
#6294=CARTESIAN_POINT('',(0.388099915049348,0.55,-0.831502973106184));
#6295=CARTESIAN_POINT('',(0.52031818912536,0.55,-1.17208286555157));
#6296=CARTESIAN_POINT('Ctrl Pts',(0.388099915049348,0.55,-0.831502973106184));
#6297=CARTESIAN_POINT('Ctrl Pts',(0.400811235892708,0.564520591324654,-0.83435608621082));
#6298=CARTESIAN_POINT('Ctrl Pts',(0.414489441774858,0.578350901074076,-0.838641228510082));
#6299=CARTESIAN_POINT('Ctrl Pts',(0.442060797330418,0.603582622702572,-0.85072830691315));
#6300=CARTESIAN_POINT('Ctrl Pts',(0.456158463572915,0.615143118816555,-0.858605324728243));
#6301=CARTESIAN_POINT('Ctrl Pts',(0.484752922098353,0.635707573307249,-0.879540531101799));
#6302=CARTESIAN_POINT('Ctrl Pts',(0.499051049160274,0.644312375876114,-0.892876836196423));
#6303=CARTESIAN_POINT('Ctrl Pts',(0.52379576928235,0.655446685849628,-0.923864041185002));
#6304=CARTESIAN_POINT('Ctrl Pts',(0.533985305944486,0.658130838683679,-0.940643830369111));
#6305=CARTESIAN_POINT('Ctrl Pts',(0.550361643571044,0.657849180985917,-0.9785497830379));
#6306=CARTESIAN_POINT('Ctrl Pts',(0.555779214799253,0.654458884420129,-0.998971235859073));
#6307=CARTESIAN_POINT('Ctrl Pts',(0.561389818753197,0.64103073977944,-1.04471484600978));
#6308=CARTESIAN_POINT('Ctrl Pts',(0.559917035408428,0.629849556228346,-1.06921795983998));
#6309=CARTESIAN_POINT('Ctrl Pts',(0.548343966268834,0.597265816764751,-1.12384601890666));
#6310=CARTESIAN_POINT('Ctrl Pts',(0.534981138426803,0.574166902399579,-1.15107608347657));
#6311=CARTESIAN_POINT('Ctrl Pts',(0.52031818912536,0.55,-1.17208286555157));
#6312=CARTESIAN_POINT('',(0.174765758038764,0.55,-0.900819442598166));
#6313=CARTESIAN_POINT('Origin',(0.339918693812442,0.55,-1.04616216792467));
#6314=CARTESIAN_POINT('',(0.119918693812442,0.652623283223421,-1.04616216792467));
#6315=CARTESIAN_POINT('Ctrl Pts',(0.119918693812442,0.652623283223421,-1.04616216792467));
#6316=CARTESIAN_POINT('Ctrl Pts',(0.119918693812442,0.651548657113519,-1.04149771220363));
#6317=CARTESIAN_POINT('Ctrl Pts',(0.120067055145305,0.650315309709256,-1.03685410010078));
#6318=CARTESIAN_POINT('Ctrl Pts',(0.12183667592796,0.64191056343947,-1.00894801471422));
#6319=CARTESIAN_POINT('Ctrl Pts',(0.126905360909727,0.631232140955599,-0.987436230688157));
#6320=CARTESIAN_POINT('Ctrl Pts',(0.14498964584378,0.598578363965738,-0.939719972286296));
#6321=CARTESIAN_POINT('Ctrl Pts',(0.160293285605306,0.574417013842143,-0.917264512724103));
#6322=CARTESIAN_POINT('Ctrl Pts',(0.174765758038763,0.55,-0.900819442598166));
#6323=CARTESIAN_POINT('',(0.119918693812442,0.9,-1.04616216792467));
#6324=CARTESIAN_POINT('',(0.119918693812442,0.,-1.04616216792467));
#6325=CARTESIAN_POINT('Origin',(0.339918693812442,0.9,-1.04616216792467));
#6326=CARTESIAN_POINT('',(0.267986765351098,0.55,-1.25407031511432));
#6327=CARTESIAN_POINT('Ctrl Pts',(0.267986765351098,0.55,-1.25407031511432));
#6328=CARTESIAN_POINT('Ctrl Pts',(0.253293148857989,0.564667428121554,-1.24898662703038));
#6329=CARTESIAN_POINT('Ctrl Pts',(0.238057625599671,0.578482229661416,-1.2419316754898));
#6330=CARTESIAN_POINT('Ctrl Pts',(0.208963044113739,0.603467206297433,-1.22375112901188));
#6331=CARTESIAN_POINT('Ctrl Pts',(0.194942594271843,0.614783224033247,-1.21267059279651));
#6332=CARTESIAN_POINT('Ctrl Pts',(0.167829116505891,0.635319330100661,-1.18473227113195));
#6333=CARTESIAN_POINT('Ctrl Pts',(0.155029153917438,0.644168216758556,-1.16745023332297));
#6334=CARTESIAN_POINT('Ctrl Pts',(0.135809963569082,0.655254671849834,-1.13051582480638));
#6335=CARTESIAN_POINT('Ctrl Pts',(0.129007044228756,0.658058624819753,-1.11187531830365));
#6336=CARTESIAN_POINT('Ctrl Pts',(0.121501840920505,0.657952259751555,-1.07686180187776));
#6337=CARTESIAN_POINT('Ctrl Pts',(0.119918693812442,0.656134080516753,-1.06140091782046));
#6338=CARTESIAN_POINT('Ctrl Pts',(0.119918693812442,0.652623283223421,-1.04616216792467));
#6339=CARTESIAN_POINT('Origin',(0.339918693812442,0.55,-1.04616216792467));
#6340=CARTESIAN_POINT('Origin',(-0.889918693812442,0.,-0.64656377752172));
#6341=CARTESIAN_POINT('',(-0.670876851625708,0.55,-0.626053502744384));
#6342=CARTESIAN_POINT('',(-0.953929883998579,0.55,-0.857045528585688));
#6343=CARTESIAN_POINT('Ctrl Pts',(-0.670876851625708,0.55,-0.626053502744384));
#6344=CARTESIAN_POINT('Ctrl Pts',(-0.669661497485836,0.564530296745674,
-0.639033017285112));
#6345=CARTESIAN_POINT('Ctrl Pts',(-0.669510740703862,0.578369513099121,
-0.653376521307855));
#6346=CARTESIAN_POINT('Ctrl Pts',(-0.672482969531502,0.603533376354093,
-0.68325868771487));
#6347=CARTESIAN_POINT('Ctrl Pts',(-0.675592903940688,0.615031149045687,
-0.699004528749127));
#6348=CARTESIAN_POINT('Ctrl Pts',(-0.686609461544843,0.635610628918897,
-0.732627526493686));
#6349=CARTESIAN_POINT('Ctrl Pts',(-0.694884092102898,0.644260777278176,
-0.750408507220998));
#6350=CARTESIAN_POINT('Ctrl Pts',(-0.716725112096974,0.655427509796643,
-0.783571551911549));
#6351=CARTESIAN_POINT('Ctrl Pts',(-0.729520363220727,0.65812029334222,-0.798445101607854));
#6352=CARTESIAN_POINT('Ctrl Pts',(-0.760487823778074,0.657862066752901,
-0.825743319709736));
#6353=CARTESIAN_POINT('Ctrl Pts',(-0.778230186437556,0.654483119781693,
-0.837216662588005));
#6354=CARTESIAN_POINT('Ctrl Pts',(-0.820018109421027,0.641069161130152,
-0.856722945878246));
#6355=CARTESIAN_POINT('Ctrl Pts',(-0.843800606133157,0.629882880868174,
-0.862908527531438));
#6356=CARTESIAN_POINT('Ctrl Pts',(-0.899368376134036,0.597285070273299,
-0.868796870135415));
#6357=CARTESIAN_POINT('Ctrl Pts',(-0.92940946533079,0.574177434161681,-0.864502617738803));
#6358=CARTESIAN_POINT('Ctrl Pts',(-0.95392988399858,0.55,-0.857045528585688));
#6359=CARTESIAN_POINT('',(-0.802724611619556,0.55,-0.444580629634229));
#6360=CARTESIAN_POINT('Origin',(-0.889918693812442,0.55,-0.64656377752172));
#6361=CARTESIAN_POINT('',(-1.10987928032073,0.55,-0.642399598979491));
#6362=CARTESIAN_POINT('Ctrl Pts',(-1.10987928032073,0.55,-0.642399598979491));
#6363=CARTESIAN_POINT('Ctrl Pts',(-1.10958615470441,0.564609024168173,-0.626916093209465));
#6364=CARTESIAN_POINT('Ctrl Pts',(-1.10759949863652,0.57837155464205,-0.610317305256214));
#6365=CARTESIAN_POINT('Ctrl Pts',(-1.09937906630242,0.603238798649671,-0.577213727602755));
#6366=CARTESIAN_POINT('Ctrl Pts',(-1.09324919553707,0.614494006479294,-0.5605724935452));
#6367=CARTESIAN_POINT('Ctrl Pts',(-1.07518267284658,0.635086936255166,-0.526160358808756));
#6368=CARTESIAN_POINT('Ctrl Pts',(-1.06268941040781,0.644016986499168,-0.508543409408808));
#6369=CARTESIAN_POINT('Ctrl Pts',(-1.03345553095711,0.655200788127591,-0.478711490622469));
#6370=CARTESIAN_POINT('Ctrl Pts',(-1.0178159360962,0.658037254761758,-0.466436266197514));
#6371=CARTESIAN_POINT('Ctrl Pts',(-0.982652377717061,0.657961095551765,
-0.446004761419876));
#6372=CARTESIAN_POINT('Ctrl Pts',(-0.963865544104577,0.654904186336904,
-0.438426323310487));
#6373=CARTESIAN_POINT('Ctrl Pts',(-0.922132837036694,0.642003792826706,
-0.427684817450471));
#6374=CARTESIAN_POINT('Ctrl Pts',(-0.900086381736092,0.631337654594768,
-0.425835547406595));
#6375=CARTESIAN_POINT('Ctrl Pts',(-0.84902407335286,0.598671631847171,-0.428254106385369));
#6376=CARTESIAN_POINT('Ctrl Pts',(-0.822877500049853,0.574466130169061,
-0.435880831514466));
#6377=CARTESIAN_POINT('Ctrl Pts',(-0.802724611619556,0.55,-0.444580629634229));
#6378=CARTESIAN_POINT('',(-1.10991869381244,0.55,-0.64656377752172));
#6379=CARTESIAN_POINT('Origin',(-0.889918693812442,0.55,-0.64656377752172));
#6380=CARTESIAN_POINT('',(-1.10991869381244,0.9,-0.64656377752172));
#6381=CARTESIAN_POINT('',(-1.10991869381244,0.,-0.64656377752172));
#6382=CARTESIAN_POINT('Origin',(-0.889918693812442,0.9,-0.64656377752172));
#6383=CARTESIAN_POINT('Origin',(-0.889918693812442,0.55,-0.64656377752172));
#6384=CARTESIAN_POINT('Origin',(1.1,0.,0.));
#6385=CARTESIAN_POINT('',(0.910735790157152,0.55,0.112156403618172));
#6386=CARTESIAN_POINT('',(1.27550420984285,0.55,0.132658480043447));
#6387=CARTESIAN_POINT('Ctrl Pts',(0.910735790157152,0.55,0.112156403618172));
#6388=CARTESIAN_POINT('Ctrl Pts',(0.917376089752458,0.564517997495034,0.123361925688083));
#6389=CARTESIAN_POINT('Ctrl Pts',(0.925676503375737,0.578345926844045,0.135044303040797));
#6390=CARTESIAN_POINT('Ctrl Pts',(0.945705763566752,0.603597412340976,0.157548233557299));
#6391=CARTESIAN_POINT('Ctrl Pts',(0.957575956315956,0.615176011910307,0.168539952403237));
#6392=CARTESIAN_POINT('Ctrl Pts',(0.986343324120607,0.635735932391,0.189265250815529));
#6393=CARTESIAN_POINT('Ctrl Pts',(1.00343254919411,0.644327528980788,0.198729556237649));
#6394=CARTESIAN_POINT('Ctrl Pts',(1.04053658704398,0.65545235887726,0.21267781162389));
#6395=CARTESIAN_POINT('Ctrl Pts',(1.05964780090184,0.658133955563747,0.217181471497843));
#6396=CARTESIAN_POINT('Ctrl Pts',(1.1007627783985,0.657845346648502,0.221036398352684));
#6397=CARTESIAN_POINT('Ctrl Pts',(1.12185832284616,0.65445169739566,0.219874810080966));
#6398=CARTESIAN_POINT('Ctrl Pts',(1.16708666484378,0.641019397008994,0.211069922924208));
#6399=CARTESIAN_POINT('Ctrl Pts',(1.18992721371268,0.629839760817717,0.202098025620397));
#6400=CARTESIAN_POINT('Ctrl Pts',(1.23829403807689,0.597260212402137,0.174213524003119));
#6401=CARTESIAN_POINT('Ctrl Pts',(1.2600586328202,0.574163836961989,0.153092633895046));
#6402=CARTESIAN_POINT('Ctrl Pts',(1.27550420984285,0.55,0.132658480043447));
#6403=CARTESIAN_POINT('',(0.88,0.55,2.69422295812418E-17));
#6404=CARTESIAN_POINT('Origin',(1.1,0.55,0.));
#6405=CARTESIAN_POINT('',(0.88,0.9,2.69422295812418E-17));
#6406=CARTESIAN_POINT('',(0.88,0.,2.69422295812418E-17));
#6407=CARTESIAN_POINT('Origin',(1.1,0.9,0.));
#6408=CARTESIAN_POINT('',(0.910735790157152,0.55,-0.112156403618172));
#6409=CARTESIAN_POINT('Origin',(1.1,0.55,0.));
#6410=CARTESIAN_POINT('',(1.27550420984285,0.55,-0.132658480043447));
#6411=CARTESIAN_POINT('Ctrl Pts',(1.27550420984285,0.55,-0.132658480043447));
#6412=CARTESIAN_POINT('Ctrl Pts',(1.26611782177473,0.56468453723726,-0.145076462072448));
#6413=CARTESIAN_POINT('Ctrl Pts',(1.25468431627751,0.578514647841062,-0.157400492027332));
#6414=CARTESIAN_POINT('Ctrl Pts',(1.22835219222699,0.603533958896828,-0.179483010322185));
#6415=CARTESIAN_POINT('Ctrl Pts',(1.21344338101808,0.614867643252025,-0.189407731207313));
#6416=CARTESIAN_POINT('Ctrl Pts',(1.17846267135551,0.635387178695068,-0.206540975098487));
#6417=CARTESIAN_POINT('Ctrl Pts',(1.15809147022147,0.644212495667266,-0.213351934557227));
#6418=CARTESIAN_POINT('Ctrl Pts',(1.11706033563968,0.65527050791581,-0.220191916744403));
#6419=CARTESIAN_POINT('Ctrl Pts',(1.09724086630217,0.658064897233583,-0.220893276198431));
#6420=CARTESIAN_POINT('Ctrl Pts',(1.05683477389847,0.657931008613642,-0.216703862540943));
#6421=CARTESIAN_POINT('Ctrl Pts',(1.03718465931368,0.654841874466928,-0.211762979306541));
#6422=CARTESIAN_POINT('Ctrl Pts',(0.997159417898573,0.641882889790503,-0.195877882014933));
#6423=CARTESIAN_POINT('Ctrl Pts',(0.978275892037171,0.631200912596756,-0.184408191234793));
#6424=CARTESIAN_POINT('Ctrl Pts',(0.938511832204562,0.598550867972523,-0.1524716629431));
#6425=CARTESIAN_POINT('Ctrl Pts',(0.921897120244161,0.57440253785522,-0.130991175878743));
#6426=CARTESIAN_POINT('Ctrl Pts',(0.910735790157152,0.55,-0.112156403618172));
#6427=CARTESIAN_POINT('Origin',(1.1,0.55,0.));
#6428=CARTESIAN_POINT('Origin',(-0.339918693812442,0.,1.04616216792467));
#6429=CARTESIAN_POINT('',(-0.388099915049348,0.55,0.831502973106184));
#6430=CARTESIAN_POINT('',(-0.559918693812442,0.63912556124056,1.04616216792335));
#6431=CARTESIAN_POINT('Ctrl Pts',(-0.388099915049348,0.55,0.831502973106184));
#6432=CARTESIAN_POINT('Ctrl Pts',(-0.400811235892709,0.564520591324655,
0.83435608621082));
#6433=CARTESIAN_POINT('Ctrl Pts',(-0.414489441774859,0.578350901074077,
0.838641228510082));
#6434=CARTESIAN_POINT('Ctrl Pts',(-0.442060797330417,0.603582622702572,
0.85072830691315));
#6435=CARTESIAN_POINT('Ctrl Pts',(-0.456158463572915,0.615143118816555,
0.858605324728243));
#6436=CARTESIAN_POINT('Ctrl Pts',(-0.484752922098353,0.635707573307249,
0.879540531101799));
#6437=CARTESIAN_POINT('Ctrl Pts',(-0.499051049160275,0.644312375876114,
0.892876836196423));
#6438=CARTESIAN_POINT('Ctrl Pts',(-0.523795769282349,0.655446685849627,
0.923864041185001));
#6439=CARTESIAN_POINT('Ctrl Pts',(-0.533985305944486,0.658130838683679,
0.94064383036911));
#6440=CARTESIAN_POINT('Ctrl Pts',(-0.550361643571044,0.657849180985917,
0.978549783037899));
#6441=CARTESIAN_POINT('Ctrl Pts',(-0.555779214799254,0.654458884420129,
0.998971235859072));
#6442=CARTESIAN_POINT('Ctrl Pts',(-0.559392545156816,0.645810916558875,
1.02843094760825));
#6443=CARTESIAN_POINT('Ctrl Pts',(-0.559918693812336,0.642672103940655,
1.03737495240447));
#6444=CARTESIAN_POINT('Ctrl Pts',(-0.559918693812442,0.63912556124056,1.04616216792202));
#6445=CARTESIAN_POINT('',(-0.174765758038764,0.55,0.900819442598166));
#6446=CARTESIAN_POINT('Origin',(-0.339918693812442,0.55,1.04616216792467));
#6447=CARTESIAN_POINT('',(-0.267986765351098,0.55,1.25407031511432));
#6448=CARTESIAN_POINT('Ctrl Pts',(-0.267986765351098,0.55,1.25407031511432));
#6449=CARTESIAN_POINT('Ctrl Pts',(-0.253293148857989,0.564667428121554,
1.24898662703038));
#6450=CARTESIAN_POINT('Ctrl Pts',(-0.238057625599671,0.578482229661416,
1.2419316754898));
#6451=CARTESIAN_POINT('Ctrl Pts',(-0.208963044113738,0.603467206297434,
1.22375112901188));
#6452=CARTESIAN_POINT('Ctrl Pts',(-0.194942594271843,0.614783224033247,
1.21267059279651));
#6453=CARTESIAN_POINT('Ctrl Pts',(-0.16782911650589,0.635319330100662,1.18473227113195));
#6454=CARTESIAN_POINT('Ctrl Pts',(-0.155029153917438,0.644168216758557,
1.16745023332297));
#6455=CARTESIAN_POINT('Ctrl Pts',(-0.135809963569082,0.655254671849834,
1.13051582480638));
#6456=CARTESIAN_POINT('Ctrl Pts',(-0.129007044228756,0.658058624819753,
1.11187531830365));
#6457=CARTESIAN_POINT('Ctrl Pts',(-0.120490750673683,0.657937930401817,
1.07214483106283));
#6458=CARTESIAN_POINT('Ctrl Pts',(-0.119110975535071,0.654856173275339,
1.05193102477361));
#6459=CARTESIAN_POINT('Ctrl Pts',(-0.121836675927961,0.64191056343947,1.00894801471422));
#6460=CARTESIAN_POINT('Ctrl Pts',(-0.126905360909727,0.631232140955598,
0.987436230688157));
#6461=CARTESIAN_POINT('Ctrl Pts',(-0.14498964584378,0.598578363965739,0.939719972286297));
#6462=CARTESIAN_POINT('Ctrl Pts',(-0.160293285605306,0.574417013842144,
0.917264512724103));
#6463=CARTESIAN_POINT('Ctrl Pts',(-0.174765758038764,0.55,0.900819442598166));
#6464=CARTESIAN_POINT('',(-0.52031818912536,0.55,1.17208286555157));
#6465=CARTESIAN_POINT('Origin',(-0.339918693812442,0.55,1.04616216792467));
#6466=CARTESIAN_POINT('Ctrl Pts',(-0.559918693812442,0.63912556124056,1.04616216792202));
#6467=CARTESIAN_POINT('Ctrl Pts',(-0.559918693812632,0.632745440529119,
1.0619700970689));
#6468=CARTESIAN_POINT('Ctrl Pts',(-0.558211019996387,0.625046304728133,
1.07727082028465));
#6469=CARTESIAN_POINT('Ctrl Pts',(-0.548343966268834,0.59726581676475,1.12384601890666));
#6470=CARTESIAN_POINT('Ctrl Pts',(-0.534981138426803,0.574166902399578,
1.15107608347657));
#6471=CARTESIAN_POINT('Ctrl Pts',(-0.52031818912536,0.55,1.17208286555157));
#6472=CARTESIAN_POINT('',(-0.559918693812442,0.9,1.04616216792467));
#6473=CARTESIAN_POINT('',(-0.559918693812442,0.,1.04616216792467));
#6474=CARTESIAN_POINT('Origin',(-0.339918693812442,0.9,1.04616216792467));
#6475=CARTESIAN_POINT('Origin',(0.889918693812442,0.,0.64656377752172));
#6476=CARTESIAN_POINT('',(0.670876851625708,0.55,0.626053502744384));
#6477=CARTESIAN_POINT('',(0.669918693812442,0.571311877390354,0.646563777525436));
#6478=CARTESIAN_POINT('Ctrl Pts',(0.670876851625708,0.55,0.626053502744384));
#6479=CARTESIAN_POINT('Ctrl Pts',(0.670266054477489,0.55730245080333,0.632576581250196));
#6480=CARTESIAN_POINT('Ctrl Pts',(0.669918693812202,0.564427939654626,0.639446501589323));
#6481=CARTESIAN_POINT('Ctrl Pts',(0.669918693812442,0.571311877390354,0.646563777529151));
#6482=CARTESIAN_POINT('',(0.802724611619556,0.55,0.444580629634229));
#6483=CARTESIAN_POINT('Origin',(0.889918693812442,0.55,0.64656377752172));
#6484=CARTESIAN_POINT('',(1.10987928032073,0.55,0.642399598979491));
#6485=CARTESIAN_POINT('Ctrl Pts',(1.10987928032073,0.55,0.642399598979492));
#6486=CARTESIAN_POINT('Ctrl Pts',(1.10958615470441,0.564609024168173,0.626916093209465));
#6487=CARTESIAN_POINT('Ctrl Pts',(1.10759949863652,0.57837155464205,0.610317305256213));
#6488=CARTESIAN_POINT('Ctrl Pts',(1.09937906630242,0.60323879864967,0.577213727602756));
#6489=CARTESIAN_POINT('Ctrl Pts',(1.09324919553707,0.614494006479294,0.560572493545201));
#6490=CARTESIAN_POINT('Ctrl Pts',(1.07518267284658,0.635086936255167,0.526160358808754));
#6491=CARTESIAN_POINT('Ctrl Pts',(1.06268941040781,0.644016986499169,0.508543409408807));
#6492=CARTESIAN_POINT('Ctrl Pts',(1.03345553095711,0.655200788127591,0.478711490622469));
#6493=CARTESIAN_POINT('Ctrl Pts',(1.0178159360962,0.658037254761758,0.466436266197514));
#6494=CARTESIAN_POINT('Ctrl Pts',(0.982652377717061,0.657961095551765,0.446004761419876));
#6495=CARTESIAN_POINT('Ctrl Pts',(0.963865544104577,0.654904186336904,0.438426323310488));
#6496=CARTESIAN_POINT('Ctrl Pts',(0.922132837036694,0.642003792826706,0.427684817450471));
#6497=CARTESIAN_POINT('Ctrl Pts',(0.900086381736093,0.631337654594768,0.425835547406595));
#6498=CARTESIAN_POINT('Ctrl Pts',(0.849024073352859,0.59867163184717,0.428254106385369));
#6499=CARTESIAN_POINT('Ctrl Pts',(0.822877500049851,0.57446613016906,0.435880831514467));
#6500=CARTESIAN_POINT('Ctrl Pts',(0.802724611619556,0.55,0.444580629634229));
#6501=CARTESIAN_POINT('',(0.953929883998579,0.55,0.857045528585688));
#6502=CARTESIAN_POINT('Origin',(0.889918693812442,0.55,0.64656377752172));
#6503=CARTESIAN_POINT('Ctrl Pts',(0.669918693812442,0.571311877390354,0.646563777529151));
#6504=CARTESIAN_POINT('Ctrl Pts',(0.66991869381268,0.57812548596788,0.65360834043107));
#6505=CARTESIAN_POINT('Ctrl Pts',(0.670258663808197,0.58470167519502,0.66089598362366));
#6506=CARTESIAN_POINT('Ctrl Pts',(0.672482969531502,0.603533376354093,0.683258687714869));
#6507=CARTESIAN_POINT('Ctrl Pts',(0.675592903940687,0.615031149045687,0.699004528749127));
#6508=CARTESIAN_POINT('Ctrl Pts',(0.686609461544844,0.635610628918897,0.732627526493686));
#6509=CARTESIAN_POINT('Ctrl Pts',(0.694884092102898,0.644260777278176,0.750408507220998));
#6510=CARTESIAN_POINT('Ctrl Pts',(0.716725112096974,0.655427509796644,0.783571551911549));
#6511=CARTESIAN_POINT('Ctrl Pts',(0.729520363220728,0.65812029334222,0.798445101607854));
#6512=CARTESIAN_POINT('Ctrl Pts',(0.760487823778074,0.657862066752901,0.825743319709735));
#6513=CARTESIAN_POINT('Ctrl Pts',(0.778230186437555,0.654483119781693,0.837216662588005));
#6514=CARTESIAN_POINT('Ctrl Pts',(0.820018109421027,0.641069161130152,0.856722945878246));
#6515=CARTESIAN_POINT('Ctrl Pts',(0.843800606133156,0.629882880868174,0.862908527531438));
#6516=CARTESIAN_POINT('Ctrl Pts',(0.899368376134038,0.597285070273298,0.868796870135415));
#6517=CARTESIAN_POINT('Ctrl Pts',(0.929409465330792,0.574177434161679,0.864502617738802));
#6518=CARTESIAN_POINT('Ctrl Pts',(0.95392988399858,0.55,0.857045528585688));
#6519=CARTESIAN_POINT('',(0.669918693812442,0.9,0.64656377752172));
#6520=CARTESIAN_POINT('',(0.669918693812442,0.,0.64656377752172));
#6521=CARTESIAN_POINT('Origin',(0.889918693812442,0.9,0.64656377752172));
#6522=CARTESIAN_POINT('Origin',(0.339918693812442,0.,1.04616216792467));
#6523=CARTESIAN_POINT('',(0.174765758038764,0.55,0.900819442598166));
#6524=CARTESIAN_POINT('',(0.119918693812442,0.652623283223421,1.04616216792467));
#6525=CARTESIAN_POINT('Ctrl Pts',(0.174765758038763,0.55,0.900819442598166));
#6526=CARTESIAN_POINT('Ctrl Pts',(0.16615910126156,0.564520591324654,0.910599186515576));
#6527=CARTESIAN_POINT('Ctrl Pts',(0.157611943697822,0.578350901074076,0.922105787154341));
#6528=CARTESIAN_POINT('Ctrl Pts',(0.142410854924047,0.603582622702572,0.948090475176036));
#6529=CARTESIAN_POINT('Ctrl Pts',(0.135635598256597,0.615143118816555,0.962749516762522));
#6530=CARTESIAN_POINT('Ctrl Pts',(0.124807600924644,0.635707573307249,0.996493855518017));
#6531=CARTESIAN_POINT('Ctrl Pts',(0.12107905659851,0.644312375876114,1.01568738120414));
#6532=CARTESIAN_POINT('Ctrl Pts',(0.119995150322276,0.65099826710225,1.03947451044843));
#6533=CARTESIAN_POINT('Ctrl Pts',(0.119918693812442,0.651851819062756,1.04281359823645));
#6534=CARTESIAN_POINT('Ctrl Pts',(0.119918693812442,0.652623283223421,1.04616216792467));
#6535=CARTESIAN_POINT('',(0.388099915049348,0.55,0.831502973106184));
#6536=CARTESIAN_POINT('Origin',(0.339918693812442,0.55,1.04616216792467));
#6537=CARTESIAN_POINT('',(0.52031818912536,0.55,1.17208286555157));
#6538=CARTESIAN_POINT('Ctrl Pts',(0.52031818912536,0.55,1.17208286555157));
#6539=CARTESIAN_POINT('Ctrl Pts',(0.529217457694123,0.564667428121555,1.15933338442007));
#6540=CARTESIAN_POINT('Ctrl Pts',(0.537396458457103,0.578482229661417,1.14467059284705));
#6541=CARTESIAN_POINT('Ctrl Pts',(0.550248212225113,0.603467206297435,1.11286085586034));
#6542=CARTESIAN_POINT('Ctrl Pts',(0.555078018641098,0.614783224033248,1.09565550010774));
#6543=CARTESIAN_POINT('Ctrl Pts',(0.560591549482129,0.635319330100661,1.05711602071761));
#6544=CARTESIAN_POINT('Ctrl Pts',(0.56078880978987,0.644168216758556,1.03561092919333));
#6545=CARTESIAN_POINT('Ctrl Pts',(0.554627960771623,0.655254671849834,0.994433608378459));
#6546=CARTESIAN_POINT('Ctrl Pts',(0.549175023311743,0.658058624819753,0.975354466173215));
#6547=CARTESIAN_POINT('Ctrl Pts',(0.532711855060331,0.657937930401817,0.938206075044727));
#6548=CARTESIAN_POINT('Ctrl Pts',(0.521946739366385,0.654856173275339,0.921041750757787));
#6549=CARTESIAN_POINT('Ctrl Pts',(0.494476822014916,0.64191056343947,0.887869891643463));
#6550=CARTESIAN_POINT('Ctrl Pts',(0.477731860324512,0.631232140955599,0.873445791067851));
#6551=CARTESIAN_POINT('Ctrl Pts',(0.435054453498551,0.598578363965736,0.84547220309525));
#6552=CARTESIAN_POINT('Ctrl Pts',(0.409474560891576,0.57441701384214,0.836300608451158));
#6553=CARTESIAN_POINT('Ctrl Pts',(0.388099915049349,0.55,0.831502973106184));
#6554=CARTESIAN_POINT('',(0.267986765351098,0.55,1.25407031511432));
#6555=CARTESIAN_POINT('Origin',(0.339918693812442,0.55,1.04616216792467));
#6556=CARTESIAN_POINT('Ctrl Pts',(0.119918693812442,0.652623283223421,1.04616216792467));
#6557=CARTESIAN_POINT('Ctrl Pts',(0.119918693812442,0.656293518143051,1.0620929629339));
#6558=CARTESIAN_POINT('Ctrl Pts',(0.121649354618456,0.658107263715709,1.07823803146977));
#6559=CARTESIAN_POINT('Ctrl Pts',(0.129925208402575,0.657849180985917,1.11515786183808));
#6560=CARTESIAN_POINT('Ctrl Pts',(0.137545730009388,0.654458884420129,1.13486353269143));
#6561=CARTESIAN_POINT('Ctrl Pts',(0.15989407549514,0.64103073977944,1.17516872094799));
#6562=CARTESIAN_POINT('Ctrl Pts',(0.175488151194729,0.629849556228346,1.19412647612185));
#6563=CARTESIAN_POINT('Ctrl Pts',(0.21696052828649,0.597265816764751,1.23151902491249));
#6564=CARTESIAN_POINT('Ctrl Pts',(0.24377671347677,0.574166902399579,1.24569413677302));
#6565=CARTESIAN_POINT('Ctrl Pts',(0.267986765351098,0.55,1.25407031511432));
#6566=CARTESIAN_POINT('',(0.119918693812442,0.9,1.04616216792467));
#6567=CARTESIAN_POINT('',(0.119918693812442,0.,1.04616216792467));
#6568=CARTESIAN_POINT('Origin',(0.339918693812442,0.9,1.04616216792467));
#6569=CARTESIAN_POINT('Origin',(-0.889918693812442,0.,0.646563777521721));
#6570=CARTESIAN_POINT('',(-0.802724611619556,0.55,0.444580629634229));
#6571=CARTESIAN_POINT('',(-1.10987928032073,0.55,0.642399598979491));
#6572=CARTESIAN_POINT('Ctrl Pts',(-0.802724611619556,0.55,0.444580629634229));
#6573=CARTESIAN_POINT('Ctrl Pts',(-0.814693298418458,0.564530296745673,
0.439413868588077));
#6574=CARTESIAN_POINT('Ctrl Pts',(-0.828288194978147,0.578369513099121,
0.434838103866291));
#6575=CARTESIAN_POINT('Ctrl Pts',(-0.857626293279466,0.603533376354093,
0.428430764212231));
#6576=CARTESIAN_POINT('Ctrl Pts',(-0.873562500583475,0.615031149045687,
0.426522755127025));
#6577=CARTESIAN_POINT('Ctrl Pts',(-0.908944175205009,0.635610628918897,
0.426610046318699));
#6578=CARTESIAN_POINT('Ctrl Pts',(-0.928411894256451,0.644260777278176,
0.428985062409479));
#6579=CARTESIAN_POINT('Ctrl Pts',(-0.96670107036224,0.655427509796644,0.439509162402782));
#6580=CARTESIAN_POINT('Ctrl Pts',(-0.984800606765885,0.65812029334222,0.447081989738822));
#6581=CARTESIAN_POINT('Ctrl Pts',(-1.02033222655978,0.657862066752901,0.468098181585364));
#6582=CARTESIAN_POINT('Ctrl Pts',(-1.03672671564999,0.654483119781693,0.48142671327546));
#6583=CARTESIAN_POINT('Ctrl Pts',(-1.0681914718434,0.641069161130152,0.515141616697554));
#6584=CARTESIAN_POINT('Ctrl Pts',(-1.08142350523446,0.629882880868174,0.535848665318463));
#6585=CARTESIAN_POINT('Ctrl Pts',(-1.10419503710793,0.597285070273303,0.586877157140452));
#6586=CARTESIAN_POINT('Ctrl Pts',(-1.10939416747485,0.574177434161687,0.616774927746317));
#6587=CARTESIAN_POINT('Ctrl Pts',(-1.10987928032073,0.55,0.642399598979492));
#6588=CARTESIAN_POINT('',(-0.670876851625708,0.55,0.626053502744384));
#6589=CARTESIAN_POINT('Origin',(-0.889918693812442,0.55,0.646563777521721));
#6590=CARTESIAN_POINT('',(-0.953929883998579,0.55,0.857045528585689));
#6591=CARTESIAN_POINT('Ctrl Pts',(-0.95392988399858,0.55,0.857045528585688));
#6592=CARTESIAN_POINT('Ctrl Pts',(-0.939113614143975,0.564609024168171,
0.861551415973636));
#6593=CARTESIAN_POINT('Ctrl Pts',(-0.922713318211477,0.57837155464205,0.864791301338213));
#6594=CARTESIAN_POINT('Ctrl Pts',(-0.888689691679124,0.603238798649673,
0.867202773669637));
#6595=CARTESIAN_POINT('Ctrl Pts',(-0.870968703349679,0.614494006479295,
0.866515344265355));
#6596=CARTESIAN_POINT('Ctrl Pts',(-0.832657955828337,0.635086936255166,
0.859966994580058));
#6597=CARTESIAN_POINT('Ctrl Pts',(-0.812042610895507,0.644016986499169,
0.853529132681505));
#6598=CARTESIAN_POINT('Ctrl Pts',(-0.774637004578397,0.655200788127591,
0.834944631013122));
#6599=CARTESIAN_POINT('Ctrl Pts',(-0.758129671802899,0.658037254761758,
0.823863745365518));
#6600=CARTESIAN_POINT('Ctrl Pts',(-0.727832018924561,0.657961095551765,
0.796734896229852));
#6601=CARTESIAN_POINT('Ctrl Pts',(-0.714819045120535,0.654904186336905,
0.781209421868766));
#6602=CARTESIAN_POINT('Ctrl Pts',(-0.691707150272296,0.642003792826706,
0.744838566725142));
#6603=CARTESIAN_POINT('Ctrl Pts',(-0.683135660593065,0.631337654594768,
0.724442597621041));
#6604=CARTESIAN_POINT('Ctrl Pts',(-0.669656725807439,0.598671631847171,
0.675132080669756));
#6605=CARTESIAN_POINT('Ctrl Pts',(-0.668830436944159,0.574466130169061,
0.647908424074824));
#6606=CARTESIAN_POINT('Ctrl Pts',(-0.670876851625708,0.55,0.626053502744384));
#6607=CARTESIAN_POINT('',(-1.10991869381244,0.55,0.646563777521721));
#6608=CARTESIAN_POINT('Origin',(-0.889918693812442,0.55,0.646563777521721));
#6609=CARTESIAN_POINT('',(-1.10991869381244,0.9,0.646563777521721));
#6610=CARTESIAN_POINT('',(-1.10991869381244,0.,0.646563777521721));
#6611=CARTESIAN_POINT('Origin',(-0.889918693812442,0.9,0.646563777521721));
#6612=CARTESIAN_POINT('Origin',(-0.889918693812442,0.55,0.646563777521721));
#6613=CARTESIAN_POINT('Origin',(-1.1,0.,1.34711147906209E-16));
#6614=CARTESIAN_POINT('',(-0.910735790157152,0.55,-0.112156403618172));
#6615=CARTESIAN_POINT('',(-1.27550420984285,0.55,-0.132658480043447));
#6616=CARTESIAN_POINT('Ctrl Pts',(-0.910735790157152,0.55,-0.112156403618172));
#6617=CARTESIAN_POINT('Ctrl Pts',(-0.917376089752458,0.564517997495035,
-0.123361925688084));
#6618=CARTESIAN_POINT('Ctrl Pts',(-0.925676503375737,0.578345926844046,
-0.135044303040797));
#6619=CARTESIAN_POINT('Ctrl Pts',(-0.945705763566753,0.603597412340976,
-0.157548233557299));
#6620=CARTESIAN_POINT('Ctrl Pts',(-0.957575956315956,0.615176011910307,
-0.168539952403237));
#6621=CARTESIAN_POINT('Ctrl Pts',(-0.986343324120607,0.635735932391,-0.189265250815529));
#6622=CARTESIAN_POINT('Ctrl Pts',(-1.00343254919411,0.644327528980788,-0.198729556237649));
#6623=CARTESIAN_POINT('Ctrl Pts',(-1.04053658704398,0.65545235887726,-0.212677811623889));
#6624=CARTESIAN_POINT('Ctrl Pts',(-1.05964780090184,0.658133955563747,-0.217181471497843));
#6625=CARTESIAN_POINT('Ctrl Pts',(-1.1007627783985,0.657845346648502,-0.221036398352684));
#6626=CARTESIAN_POINT('Ctrl Pts',(-1.12185832284616,0.65445169739566,-0.219874810080966));
#6627=CARTESIAN_POINT('Ctrl Pts',(-1.16708666484378,0.641019397008994,-0.211069922924208));
#6628=CARTESIAN_POINT('Ctrl Pts',(-1.18992721371268,0.629839760817717,-0.202098025620397));
#6629=CARTESIAN_POINT('Ctrl Pts',(-1.23829403807688,0.597260212402138,-0.174213524003119));
#6630=CARTESIAN_POINT('Ctrl Pts',(-1.2600586328202,0.57416383696199,-0.153092633895047));
#6631=CARTESIAN_POINT('Ctrl Pts',(-1.27550420984285,0.55,-0.132658480043447));
#6632=CARTESIAN_POINT('',(-0.910735790157152,0.55,0.112156403618172));
#6633=CARTESIAN_POINT('Origin',(-1.1,0.55,1.34711147906209E-16));
#6634=CARTESIAN_POINT('',(-1.27550420984285,0.55,0.132658480043447));
#6635=CARTESIAN_POINT('Ctrl Pts',(-1.27550420984285,0.55,0.132658480043447));
#6636=CARTESIAN_POINT('Ctrl Pts',(-1.26611782177473,0.56468453723726,0.145076462072449));
#6637=CARTESIAN_POINT('Ctrl Pts',(-1.25468431627751,0.578514647841062,0.157400492027332));
#6638=CARTESIAN_POINT('Ctrl Pts',(-1.22835219222699,0.603533958896827,0.179483010322184));
#6639=CARTESIAN_POINT('Ctrl Pts',(-1.21344338101808,0.614867643252025,0.189407731207314));
#6640=CARTESIAN_POINT('Ctrl Pts',(-1.17846267135551,0.635387178695069,0.206540975098488));
#6641=CARTESIAN_POINT('Ctrl Pts',(-1.15809147022147,0.644212495667266,0.213351934557227));
#6642=CARTESIAN_POINT('Ctrl Pts',(-1.11706033563968,0.65527050791581,0.220191916744403));
#6643=CARTESIAN_POINT('Ctrl Pts',(-1.09724086630217,0.658064897233583,0.220893276198431));
#6644=CARTESIAN_POINT('Ctrl Pts',(-1.05683477389847,0.657931008613642,0.216703862540943));
#6645=CARTESIAN_POINT('Ctrl Pts',(-1.03718465931368,0.654841874466928,0.211762979306541));
#6646=CARTESIAN_POINT('Ctrl Pts',(-0.997159417898573,0.641882889790503,
0.195877882014933));
#6647=CARTESIAN_POINT('Ctrl Pts',(-0.978275892037171,0.631200912596757,
0.184408191234794));
#6648=CARTESIAN_POINT('Ctrl Pts',(-0.938511832204561,0.598550867972523,
0.1524716629431));
#6649=CARTESIAN_POINT('Ctrl Pts',(-0.921897120244161,0.57440253785522,0.130991175878743));
#6650=CARTESIAN_POINT('Ctrl Pts',(-0.910735790157152,0.55,0.112156403618173));
#6651=CARTESIAN_POINT('',(-1.32,0.55,1.61653377487451E-16));
#6652=CARTESIAN_POINT('Origin',(-1.1,0.55,1.34711147906209E-16));
#6653=CARTESIAN_POINT('',(-1.32,0.9,1.61653377487451E-16));
#6654=CARTESIAN_POINT('',(-1.32,0.,1.61653377487451E-16));
#6655=CARTESIAN_POINT('Origin',(-1.1,0.9,1.34711147906209E-16));
#6656=CARTESIAN_POINT('Origin',(-1.1,0.55,1.34711147906209E-16));
#6657=CARTESIAN_POINT('Origin',(-0.339918693812442,0.,-1.04616216792467));
#6658=CARTESIAN_POINT('',(-0.174765758038764,0.55,-0.900819442598166));
#6659=CARTESIAN_POINT('',(-0.267986765351098,0.55,-1.25407031511432));
#6660=CARTESIAN_POINT('Ctrl Pts',(-0.174765758038764,0.55,-0.900819442598166));
#6661=CARTESIAN_POINT('Ctrl Pts',(-0.16615910126156,0.564520591324654,-0.910599186515576));
#6662=CARTESIAN_POINT('Ctrl Pts',(-0.157611943697822,0.578350901074076,
-0.922105787154341));
#6663=CARTESIAN_POINT('Ctrl Pts',(-0.142410854924047,0.603582622702572,
-0.948090475176037));
#6664=CARTESIAN_POINT('Ctrl Pts',(-0.135635598256598,0.615143118816555,
-0.962749516762522));
#6665=CARTESIAN_POINT('Ctrl Pts',(-0.124807600924644,0.635707573307249,
-0.996493855518017));
#6666=CARTESIAN_POINT('Ctrl Pts',(-0.12107905659851,0.644312375876114,-1.01568738120414));
#6667=CARTESIAN_POINT('Ctrl Pts',(-0.11927397960075,0.655446685849627,-1.05530113820794));
#6668=CARTESIAN_POINT('Ctrl Pts',(-0.120893383895271,0.658130838683679,
-1.07486553219761));
#6669=CARTESIAN_POINT('Ctrl Pts',(-0.129925208402575,0.657849180985917,
-1.11515786183808));
#6670=CARTESIAN_POINT('Ctrl Pts',(-0.137545730009389,0.654458884420129,
-1.13486353269143));
#6671=CARTESIAN_POINT('Ctrl Pts',(-0.15989407549514,0.64103073977944,-1.17516872094799));
#6672=CARTESIAN_POINT('Ctrl Pts',(-0.175488151194729,0.629849556228346,
-1.19412647612185));
#6673=CARTESIAN_POINT('Ctrl Pts',(-0.216960528286492,0.59726581676475,-1.2315190249125));
#6674=CARTESIAN_POINT('Ctrl Pts',(-0.243776713476771,0.574166902399578,
-1.24569413677302));
#6675=CARTESIAN_POINT('Ctrl Pts',(-0.267986765351099,0.55,-1.25407031511432));
#6676=CARTESIAN_POINT('',(-0.388099915049348,0.55,-0.831502973106184));
#6677=CARTESIAN_POINT('Origin',(-0.339918693812442,0.55,-1.04616216792467));
#6678=CARTESIAN_POINT('',(-0.559918693812442,0.639125561239885,-1.04616216792418));
#6679=CARTESIAN_POINT('Ctrl Pts',(-0.559918693812442,0.639125561239885,
-1.04616216792369));
#6680=CARTESIAN_POINT('Ctrl Pts',(-0.559918693812395,0.643427932070251,
-1.03550224841357));
#6681=CARTESIAN_POINT('Ctrl Pts',(-0.55914412823418,0.647127823162253,-1.02461835660206));
#6682=CARTESIAN_POINT('Ctrl Pts',(-0.554627960771623,0.655254671849834,
-0.994433608378459));
#6683=CARTESIAN_POINT('Ctrl Pts',(-0.549175023311743,0.658058624819753,
-0.975354466173216));
#6684=CARTESIAN_POINT('Ctrl Pts',(-0.532711855060331,0.657937930401817,
-0.938206075044727));
#6685=CARTESIAN_POINT('Ctrl Pts',(-0.521946739366384,0.654856173275339,
-0.921041750757787));
#6686=CARTESIAN_POINT('Ctrl Pts',(-0.494476822014917,0.64191056343947,-0.887869891643464));
#6687=CARTESIAN_POINT('Ctrl Pts',(-0.477731860324512,0.631232140955599,
-0.873445791067852));
#6688=CARTESIAN_POINT('Ctrl Pts',(-0.435054453498552,0.598578363965737,
-0.84547220309525));
#6689=CARTESIAN_POINT('Ctrl Pts',(-0.409474560891577,0.574417013842142,
-0.836300608451158));
#6690=CARTESIAN_POINT('Ctrl Pts',(-0.388099915049349,0.55,-0.831502973106184));
#6691=CARTESIAN_POINT('',(-0.559918693812442,0.9,-1.04616216792467));
#6692=CARTESIAN_POINT('',(-0.559918693812442,0.,-1.04616216792467));
#6693=CARTESIAN_POINT('Origin',(-0.339918693812442,0.9,-1.04616216792467));
#6694=CARTESIAN_POINT('',(-0.52031818912536,0.55,-1.17208286555157));
#6695=CARTESIAN_POINT('Ctrl Pts',(-0.52031818912536,0.55,-1.17208286555157));
#6696=CARTESIAN_POINT('Ctrl Pts',(-0.529217457694122,0.564667428121554,
-1.15933338442007));
#6697=CARTESIAN_POINT('Ctrl Pts',(-0.537396458457103,0.578482229661416,
-1.14467059284705));
#6698=CARTESIAN_POINT('Ctrl Pts',(-0.550248212225112,0.603467206297434,
-1.11286085586034));
#6699=CARTESIAN_POINT('Ctrl Pts',(-0.555078018641099,0.614783224033247,
-1.09565550010774));
#6700=CARTESIAN_POINT('Ctrl Pts',(-0.559145317472554,0.629932587049239,
-1.06722515592215));
#6701=CARTESIAN_POINT('Ctrl Pts',(-0.559918693812489,0.634829883465696,
-1.05680550414918));
#6702=CARTESIAN_POINT('Ctrl Pts',(-0.559918693812442,0.639125561239885,
-1.04616216792369));
#6703=CARTESIAN_POINT('Origin',(-0.339918693812442,0.55,-1.04616216792467));
#6704=CARTESIAN_POINT('Origin',(0.889918693812442,0.,-0.646563777521721));
#6705=CARTESIAN_POINT('',(0.802724611619556,0.55,-0.444580629634229));
#6706=CARTESIAN_POINT('',(1.10987928032073,0.55,-0.642399598979491));
#6707=CARTESIAN_POINT('Ctrl Pts',(0.802724611619556,0.55,-0.444580629634229));
#6708=CARTESIAN_POINT('Ctrl Pts',(0.814693298418457,0.564530296745673,-0.439413868588077));
#6709=CARTESIAN_POINT('Ctrl Pts',(0.828288194978146,0.578369513099121,-0.434838103866291));
#6710=CARTESIAN_POINT('Ctrl Pts',(0.857626293279466,0.603533376354093,-0.428430764212231));
#6711=CARTESIAN_POINT('Ctrl Pts',(0.873562500583474,0.615031149045687,-0.426522755127025));
#6712=CARTESIAN_POINT('Ctrl Pts',(0.908944175205009,0.635610628918897,-0.426610046318699));
#6713=CARTESIAN_POINT('Ctrl Pts',(0.928411894256451,0.644260777278176,-0.428985062409479));
#6714=CARTESIAN_POINT('Ctrl Pts',(0.96670107036224,0.655427509796644,-0.439509162402782));
#6715=CARTESIAN_POINT('Ctrl Pts',(0.984800606765885,0.65812029334222,-0.447081989738822));
#6716=CARTESIAN_POINT('Ctrl Pts',(1.02033222655978,0.657862066752901,-0.468098181585364));
#6717=CARTESIAN_POINT('Ctrl Pts',(1.03672671564999,0.654483119781693,-0.481426713275459));
#6718=CARTESIAN_POINT('Ctrl Pts',(1.0681914718434,0.641069161130152,-0.515141616697554));
#6719=CARTESIAN_POINT('Ctrl Pts',(1.08142350523446,0.629882880868174,-0.535848665318462));
#6720=CARTESIAN_POINT('Ctrl Pts',(1.10419503710794,0.597285070273298,-0.58687715714046));
#6721=CARTESIAN_POINT('Ctrl Pts',(1.10939416747485,0.574177434161679,-0.616774927746326));
#6722=CARTESIAN_POINT('Ctrl Pts',(1.10987928032073,0.55,-0.642399598979492));
#6723=CARTESIAN_POINT('',(0.670876851625708,0.55,-0.626053502744384));
#6724=CARTESIAN_POINT('Origin',(0.889918693812442,0.55,-0.646563777521721));
#6725=CARTESIAN_POINT('',(0.669918693812442,0.571311877460243,-0.646563777561565));
#6726=CARTESIAN_POINT('Ctrl Pts',(0.669918693812442,0.571311877460243,-0.646563777601409));
#6727=CARTESIAN_POINT('Ctrl Pts',(0.669918693809818,0.564304796586028,-0.639319184455347));
#6728=CARTESIAN_POINT('Ctrl Pts',(0.670277510265801,0.557165489897726,-0.632454237839258));
#6729=CARTESIAN_POINT('Ctrl Pts',(0.670876851625708,0.55,-0.626053502744384));
#6730=CARTESIAN_POINT('',(0.669918693812442,0.9,-0.646563777521721));
#6731=CARTESIAN_POINT('',(0.669918693812442,0.,-0.646563777521721));
#6732=CARTESIAN_POINT('Origin',(0.889918693812442,0.9,-0.646563777521721));
#6733=CARTESIAN_POINT('',(0.953929883998579,0.55,-0.857045528585689));
#6734=CARTESIAN_POINT('Ctrl Pts',(0.953929883998579,0.55,-0.857045528585689));
#6735=CARTESIAN_POINT('Ctrl Pts',(0.939113614143974,0.564609024168172,-0.861551415973636));
#6736=CARTESIAN_POINT('Ctrl Pts',(0.922713318211476,0.57837155464205,-0.864791301338213));
#6737=CARTESIAN_POINT('Ctrl Pts',(0.888689691679126,0.603238798649671,-0.867202773669637));
#6738=CARTESIAN_POINT('Ctrl Pts',(0.87096870334968,0.614494006479294,-0.866515344265356));
#6739=CARTESIAN_POINT('Ctrl Pts',(0.832657955828336,0.635086936255167,-0.859966994580058));
#6740=CARTESIAN_POINT('Ctrl Pts',(0.812042610895507,0.644016986499169,-0.853529132681505));
#6741=CARTESIAN_POINT('Ctrl Pts',(0.774637004578397,0.655200788127591,-0.834944631013121));
#6742=CARTESIAN_POINT('Ctrl Pts',(0.758129671802899,0.658037254761758,-0.823863745365518));
#6743=CARTESIAN_POINT('Ctrl Pts',(0.727832018924561,0.657961095551765,-0.796734896229852));
#6744=CARTESIAN_POINT('Ctrl Pts',(0.714819045120535,0.654904186336905,-0.781209421868767));
#6745=CARTESIAN_POINT('Ctrl Pts',(0.691707150272296,0.642003792826706,-0.744838566725142));
#6746=CARTESIAN_POINT('Ctrl Pts',(0.683135660593065,0.631337654594767,-0.72444259762104));
#6747=CARTESIAN_POINT('Ctrl Pts',(0.672013600394922,0.604383486686772,-0.683754327616307));
#6748=CARTESIAN_POINT('Ctrl Pts',(0.669918693818778,0.588230048762875,-0.664055407862729));
#6749=CARTESIAN_POINT('Ctrl Pts',(0.669918693812442,0.571311877460243,-0.646563777601409));
#6750=CARTESIAN_POINT('Origin',(0.889918693812442,0.55,-0.646563777521721));
#6751=CARTESIAN_POINT('Origin',(0.8,0.55,0.));
#6752=CARTESIAN_POINT('Origin',(0.,0.55,0.));
#6753=CARTESIAN_POINT('Origin',(0.,0.55,0.));
#6754=CARTESIAN_POINT('Origin',(0.,0.55,0.));
#6755=CARTESIAN_POINT('Origin',(0.,0.55,0.));
#6756=CARTESIAN_POINT('Origin',(0.,0.55,0.));
#6757=CARTESIAN_POINT('Origin',(0.,0.55,0.));
#6758=CARTESIAN_POINT('Origin',(0.,0.55,0.));
#6759=CARTESIAN_POINT('Origin',(0.,0.55,0.));
#6760=CARTESIAN_POINT('Origin',(0.,0.55,0.));
#6761=CARTESIAN_POINT('Origin',(0.,0.55,0.));
#6762=CARTESIAN_POINT('',(-0.8,0.55,-9.79717439317883E-17));
#6763=CARTESIAN_POINT('Origin',(0.,0.55,0.));
#6764=CARTESIAN_POINT('Origin',(0.,0.45,0.));
#6765=CARTESIAN_POINT('Origin',(0.,0.55,0.));
#6766=CARTESIAN_POINT('Origin',(0.,0.45,0.));
#6767=CARTESIAN_POINT('Origin',(0.,0.55,0.));
#6768=CARTESIAN_POINT('Origin',(0.,0.45,0.));
#6769=CARTESIAN_POINT('Origin',(0.,0.55,0.));
#6770=CARTESIAN_POINT('Origin',(0.,0.45,0.));
#6771=CARTESIAN_POINT('Origin',(0.,0.55,0.));
#6772=CARTESIAN_POINT('Origin',(0.,0.45,0.));
#6773=CARTESIAN_POINT('Origin',(0.,0.55,0.));
#6774=CARTESIAN_POINT('Origin',(0.,0.45,0.));
#6775=CARTESIAN_POINT('Origin',(0.,0.55,0.));
#6776=CARTESIAN_POINT('Origin',(0.,0.45,0.));
#6777=CARTESIAN_POINT('Origin',(0.,0.55,0.));
#6778=CARTESIAN_POINT('Origin',(0.,0.45,0.));
#6779=CARTESIAN_POINT('Origin',(0.,0.55,0.));
#6780=CARTESIAN_POINT('Origin',(0.,0.45,0.));
#6781=CARTESIAN_POINT('Origin',(0.,0.55,0.));
#6782=CARTESIAN_POINT('Origin',(0.,0.45,0.));
#6783=CARTESIAN_POINT('Origin',(0.,0.55,0.));
#6784=CARTESIAN_POINT('Origin',(1.4,0.9,0.));
#6785=CARTESIAN_POINT('',(-1.4,0.9,-1.71450551880629E-16));
#6786=CARTESIAN_POINT('Origin',(0.,0.9,0.));
#6787=CARTESIAN_POINT('',(-0.8,0.9,-9.79717439317883E-17));
#6788=CARTESIAN_POINT('Origin',(0.,0.9,0.));
#6789=CARTESIAN_POINT('Origin',(0.,0.725,0.));
#6790=CARTESIAN_POINT('',(-1.4,0.55,-1.71450551880629E-16));
#6791=CARTESIAN_POINT('Origin',(0.,0.55,0.));
#6792=CARTESIAN_POINT('',(-1.4,0.725,-1.71450551880629E-16));
#6793=CARTESIAN_POINT('Origin',(0.8,0.55,0.));
#6794=CARTESIAN_POINT('Origin',(0.,0.725,0.));
#6795=CARTESIAN_POINT('',(-0.8,0.725,-9.79717439317883E-17));
#6796=CARTESIAN_POINT('',(0.,0.,0.));
#6797=CARTESIAN_POINT('Origin',(1.1,0.45,0.));
#6798=CARTESIAN_POINT('',(1.1,0.45,0.2));
#6799=CARTESIAN_POINT('',(1.1,0.45,-0.2));
#6800=CARTESIAN_POINT('Origin',(1.1,0.45,0.));
#6801=CARTESIAN_POINT('Origin',(0.889918693812442,0.45,-0.64656377752172));
#6802=CARTESIAN_POINT('',(1.00747574427094,0.45,-0.484760378646731));
#6803=CARTESIAN_POINT('',(0.772361643353948,0.45,-0.80836717639671));
#6804=CARTESIAN_POINT('Origin',(0.889918693812442,0.45,-0.64656377752172));
#6805=CARTESIAN_POINT('Origin',(0.339918693812442,0.45,-1.04616216792467));
#6806=CARTESIAN_POINT('',(0.530129997071473,0.45,-0.98435876904968));
#6807=CARTESIAN_POINT('',(0.149707390553412,0.45,-1.10796556679966));
#6808=CARTESIAN_POINT('Origin',(0.339918693812442,0.45,-1.04616216792467));
#6809=CARTESIAN_POINT('Origin',(-0.339918693812442,0.45,-1.04616216792467));
#6810=CARTESIAN_POINT('',(-0.149707390553411,0.45,-1.10796556679966));
#6811=CARTESIAN_POINT('',(-0.530129997071473,0.45,-0.98435876904968));
#6812=CARTESIAN_POINT('Origin',(-0.339918693812442,0.45,-1.04616216792467));
#6813=CARTESIAN_POINT('Origin',(-0.889918693812442,0.45,-0.646563777521721));
#6814=CARTESIAN_POINT('',(-0.772361643353948,0.45,-0.80836717639671));
#6815=CARTESIAN_POINT('',(-1.00747574427094,0.45,-0.484760378646731));
#6816=CARTESIAN_POINT('Origin',(-0.889918693812442,0.45,-0.646563777521721));
#6817=CARTESIAN_POINT('Origin',(-1.1,0.45,-1.34711147906209E-16));
#6818=CARTESIAN_POINT('',(-1.1,0.45,-0.2));
#6819=CARTESIAN_POINT('',(-1.1,0.45,0.2));
#6820=CARTESIAN_POINT('Origin',(-1.1,0.45,-1.34711147906209E-16));
#6821=CARTESIAN_POINT('Origin',(-0.889918693812442,0.45,0.64656377752172));
#6822=CARTESIAN_POINT('',(-1.00747574427094,0.45,0.484760378646731));
#6823=CARTESIAN_POINT('',(-0.772361643353948,0.45,0.80836717639671));
#6824=CARTESIAN_POINT('Origin',(-0.889918693812442,0.45,0.64656377752172));
#6825=CARTESIAN_POINT('Origin',(-0.339918693812442,0.45,1.04616216792467));
#6826=CARTESIAN_POINT('',(-0.530129997071473,0.45,0.984358769049679));
#6827=CARTESIAN_POINT('',(-0.149707390553412,0.45,1.10796556679966));
#6828=CARTESIAN_POINT('Origin',(-0.339918693812442,0.45,1.04616216792467));
#6829=CARTESIAN_POINT('Origin',(0.339918693812442,0.45,1.04616216792467));
#6830=CARTESIAN_POINT('',(0.149707390553411,0.45,1.10796556679966));
#6831=CARTESIAN_POINT('',(0.530129997071473,0.45,0.98435876904968));
#6832=CARTESIAN_POINT('Origin',(0.339918693812442,0.45,1.04616216792467));
#6833=CARTESIAN_POINT('Origin',(0.889918693812442,0.45,0.646563777521721));
#6834=CARTESIAN_POINT('',(0.772361643353948,0.45,0.80836717639671));
#6835=CARTESIAN_POINT('',(1.00747574427094,0.45,0.484760378646731));
#6836=CARTESIAN_POINT('Origin',(0.889918693812442,0.45,0.646563777521721));
#6837=CARTESIAN_POINT('',(0.,0.,0.));
#6838=CARTESIAN_POINT('',(0.,0.,0.));
#6839=CARTESIAN_POINT('',(0.,0.,0.));
#6840=CARTESIAN_POINT('',(0.,0.,0.));
#6841=CARTESIAN_POINT('Origin',(0.,0.,0.));
#6842=CARTESIAN_POINT('',(-0.42,0.16,5.14351655641888E-17));
#6843=CARTESIAN_POINT('Origin',(0.,0.16,0.));
#6844=CARTESIAN_POINT('',(-0.42,0.,5.14351655641888E-17));
#6845=CARTESIAN_POINT('',(-0.42,0.,5.14351655641888E-17));
#6846=CARTESIAN_POINT('Origin',(0.,0.,0.));
#6847=CARTESIAN_POINT('Origin',(0.,0.,0.));
#6848=CARTESIAN_POINT('',(-0.8,0.16,9.79717439317883E-17));
#6849=CARTESIAN_POINT('Origin',(0.,0.16,0.));
#6850=CARTESIAN_POINT('',(-0.8,0.,9.79717439317883E-17));
#6851=CARTESIAN_POINT('',(-0.8,0.,9.79717439317883E-17));
#6852=CARTESIAN_POINT('Origin',(0.,0.,0.));
#6853=CARTESIAN_POINT('Origin',(0.,0.16,0.));
#6854=CARTESIAN_POINT('Origin',(0.,0.,0.));
#6855=CARTESIAN_POINT('',(0.,0.,0.));
#6856=CARTESIAN_POINT('Origin',(0.,0.067277284513851,0.));
#6857=CARTESIAN_POINT('',(-0.375277674973257,0.0768195421087395,0.65));
#6858=CARTESIAN_POINT('',(0.375277674973257,0.0768195421087395,0.65));
#6859=CARTESIAN_POINT('Ctrl Pts',(-0.375277674973257,0.0768195421087395,
0.65));
#6860=CARTESIAN_POINT('Ctrl Pts',(1.66533453693773E-13,-0.0315137912242439,
0.65));
#6861=CARTESIAN_POINT('Ctrl Pts',(0.375277674973257,0.0768195421087394,
0.65));
#6862=CARTESIAN_POINT('',(-0.750555349946514,0.0768195421087394,-9.19165206894919E-17));
#6863=CARTESIAN_POINT('Ctrl Pts',(-0.750555349946514,0.0768195421087394,
-9.19165206894919E-17));
#6864=CARTESIAN_POINT('Ctrl Pts',(-0.562916512459802,-0.0315137912242434,
0.325000000000144));
#6865=CARTESIAN_POINT('Ctrl Pts',(-0.375277674973257,0.0768195421087395,
0.65));
#6866=CARTESIAN_POINT('',(-0.6175,-2.77555756156289E-17,-7.5621939847349E-17));
#6867=CARTESIAN_POINT('',(-0.734027674973257,0.067277284513851,-8.98924642641573E-17));
#6868=CARTESIAN_POINT('Origin',(0.,0.,0.));
#6869=CARTESIAN_POINT('',(-0.375277674973257,0.0768195421087395,-0.65));
#6870=CARTESIAN_POINT('Ctrl Pts',(-0.375277674973257,0.0768195421087395,
-0.65));
#6871=CARTESIAN_POINT('Ctrl Pts',(-0.562916512459968,-0.0315137912242437,
-0.324999999999856));
#6872=CARTESIAN_POINT('Ctrl Pts',(-0.750555349946514,0.0768195421087395,
-9.19165206894919E-17));
#6873=CARTESIAN_POINT('',(0.375277674973257,0.0768195421087395,-0.65));
#6874=CARTESIAN_POINT('Ctrl Pts',(0.375277674973257,0.0768195421087395,
-0.65));
#6875=CARTESIAN_POINT('Ctrl Pts',(-1.66144875635155E-13,-0.0315137912242437,
-0.65));
#6876=CARTESIAN_POINT('Ctrl Pts',(-0.375277674973257,0.0768195421087395,
-0.65));
#6877=CARTESIAN_POINT('',(0.750555349946514,0.0768195421087394,0.));
#6878=CARTESIAN_POINT('Ctrl Pts',(0.750555349946514,0.0768195421087394,
0.));
#6879=CARTESIAN_POINT('Ctrl Pts',(0.562916512459802,-0.0315137912242436,
-0.325000000000144));
#6880=CARTESIAN_POINT('Ctrl Pts',(0.375277674973257,0.0768195421087395,
-0.65));
#6881=CARTESIAN_POINT('Ctrl Pts',(0.375277674973257,0.0768195421087394,
0.65));
#6882=CARTESIAN_POINT('Ctrl Pts',(0.562916512459968,-0.0315137912242439,
0.324999999999856));
#6883=CARTESIAN_POINT('Ctrl Pts',(0.750555349946514,0.0768195421087394,
0.));
#6884=CARTESIAN_POINT('Origin',(0.,0.612722715486149,0.));
#6885=CARTESIAN_POINT('',(-0.6175,0.68,-7.5621939847349E-17));
#6886=CARTESIAN_POINT('Origin',(0.,0.68,0.));
#6887=CARTESIAN_POINT('',(-0.750555349946514,0.603180457891261,-9.19165206894919E-17));
#6888=CARTESIAN_POINT('',(-0.734027674973257,0.612722715486149,-8.98924642641573E-17));
#6889=CARTESIAN_POINT('',(-0.375277674973257,0.603180457891261,0.65));
#6890=CARTESIAN_POINT('Ctrl Pts',(-0.375277674973257,0.603180457891261,
0.65));
#6891=CARTESIAN_POINT('Ctrl Pts',(-0.562916512459968,0.711513791224243,
0.324999999999856));
#6892=CARTESIAN_POINT('Ctrl Pts',(-0.750555349946514,0.603180457891261,
-9.19165206894919E-17));
#6893=CARTESIAN_POINT('',(0.375277674973257,0.603180457891261,0.65));
#6894=CARTESIAN_POINT('Ctrl Pts',(0.375277674973257,0.603180457891261,0.65));
#6895=CARTESIAN_POINT('Ctrl Pts',(-1.66755498298699E-13,0.711513791224244,
0.65));
#6896=CARTESIAN_POINT('Ctrl Pts',(-0.375277674973257,0.603180457891261,
0.65));
#6897=CARTESIAN_POINT('',(0.750555349946514,0.603180457891261,0.));
#6898=CARTESIAN_POINT('Ctrl Pts',(0.750555349946514,0.603180457891261,0.));
#6899=CARTESIAN_POINT('Ctrl Pts',(0.562916512459802,0.711513791224244,0.325000000000144));
#6900=CARTESIAN_POINT('Ctrl Pts',(0.375277674973257,0.603180457891261,0.65));
#6901=CARTESIAN_POINT('',(0.375277674973257,0.603180457891261,-0.65));
#6902=CARTESIAN_POINT('Ctrl Pts',(0.375277674973257,0.603180457891261,-0.65));
#6903=CARTESIAN_POINT('Ctrl Pts',(0.562916512459969,0.711513791224244,-0.324999999999856));
#6904=CARTESIAN_POINT('Ctrl Pts',(0.750555349946514,0.603180457891261,0.));
#6905=CARTESIAN_POINT('',(-0.375277674973257,0.603180457891261,-0.65));
#6906=CARTESIAN_POINT('Ctrl Pts',(-0.375277674973257,0.603180457891261,
-0.65));
#6907=CARTESIAN_POINT('Ctrl Pts',(1.66422431391311E-13,0.711513791224244,
-0.65));
#6908=CARTESIAN_POINT('Ctrl Pts',(0.375277674973257,0.603180457891261,-0.65));
#6909=CARTESIAN_POINT('Ctrl Pts',(-0.750555349946514,0.603180457891261,
-9.19165206894919E-17));
#6910=CARTESIAN_POINT('Ctrl Pts',(-0.562916512459802,0.711513791224244,
-0.325000000000144));
#6911=CARTESIAN_POINT('Ctrl Pts',(-0.375277674973257,0.603180457891261,
-0.65));
#6912=CARTESIAN_POINT('Origin',(0.375277674973257,0.,-0.65));
#6913=CARTESIAN_POINT('',(-0.375277674973257,0.,-0.65));
#6914=CARTESIAN_POINT('',(0.375277674973257,0.,-0.65));
#6915=CARTESIAN_POINT('Origin',(-0.375277674973257,0.,-0.65));
#6916=CARTESIAN_POINT('',(-0.750555349946514,0.,-9.19165206894919E-17));
#6917=CARTESIAN_POINT('Origin',(-0.750555349946514,0.,-9.19165206894919E-17));
#6918=CARTESIAN_POINT('',(-0.375277674973257,0.,0.65));
#6919=CARTESIAN_POINT('Origin',(0.,0.,0.));
#6920=CARTESIAN_POINT('',(-0.338975,0.68,4.15124648740974E-17));
#6921=CARTESIAN_POINT('Origin',(0.,0.68,0.));
#6922=CARTESIAN_POINT('',(-0.338975,0.,4.15124648740974E-17));
#6923=CARTESIAN_POINT('',(-0.338975,0.,4.15124648740974E-17));
#6924=CARTESIAN_POINT('Origin',(0.,0.,0.));
#6925=CARTESIAN_POINT('Origin',(-0.375277674973257,0.,0.65));
#6926=CARTESIAN_POINT('',(0.375277674973257,0.,0.65));
#6927=CARTESIAN_POINT('Origin',(0.750555349946514,0.,0.));
#6928=CARTESIAN_POINT('',(0.750555349946514,0.,0.));
#6929=CARTESIAN_POINT('Origin',(0.375277674973257,0.,0.65));
#6930=CARTESIAN_POINT('Origin',(0.,0.68,-1.11022302462516E-16));
#6931=CARTESIAN_POINT('Origin',(0.,0.,-1.11022302462516E-16));
#6932=CARTESIAN_POINT('',(0.,0.,0.));
#6933=CARTESIAN_POINT('',(0.,0.,0.));
#6934=CARTESIAN_POINT('',(-2.,0.,9.3));
#6935=CARTESIAN_POINT('',(-2.,0.,8.5));
#6936=CARTESIAN_POINT('',(-2.,0.,8.34));
#6937=CARTESIAN_POINT('',(0.,0.,0.));
#6938=CARTESIAN_POINT('',(0.,0.,0.));
#6939=CARTESIAN_POINT('Origin',(-2.,0.,8.4));
#6940=CARTESIAN_POINT('',(-2.8,-9.79717439317883E-17,8.5));
#6941=CARTESIAN_POINT('Origin',(-2.,0.,8.5));
#6942=CARTESIAN_POINT('',(-2.8,9.79717439317883E-17,9.3));
#6943=CARTESIAN_POINT('',(-2.8,-9.79717439317883E-17,8.4));
#6944=CARTESIAN_POINT('Origin',(-2.,0.,9.3));
#6945=CARTESIAN_POINT('Origin',(0.,-2.1,4.));
#6946=CARTESIAN_POINT('',(0.6,-1.5,4.));
#6947=CARTESIAN_POINT('',(-0.6,-1.5,4.));
#6948=CARTESIAN_POINT('Origin',(0.,-1.5,4.));
#6949=CARTESIAN_POINT('',(0.6,-2.,4.));
#6950=CARTESIAN_POINT('',(0.6,-2.1,4.));
#6951=CARTESIAN_POINT('',(-0.6,-2.,4.));
#6952=CARTESIAN_POINT('Origin',(0.,-2.,4.));
#6953=CARTESIAN_POINT('',(-0.6,-2.1,4.));
#6954=CARTESIAN_POINT('Origin',(0.,-2.1,4.));
#6955=CARTESIAN_POINT('',(-0.6,2.,4.));
#6956=CARTESIAN_POINT('',(-0.6,1.5,4.));
#6957=CARTESIAN_POINT('',(-0.6,-2.1,4.));
#6958=CARTESIAN_POINT('',(0.6,2.,4.));
#6959=CARTESIAN_POINT('Origin',(0.,2.,4.));
#6960=CARTESIAN_POINT('',(0.6,1.5,4.));
#6961=CARTESIAN_POINT('',(0.6,-2.1,4.));
#6962=CARTESIAN_POINT('Origin',(0.,1.5,4.));
#6963=CARTESIAN_POINT('Origin',(2.,2.,8.5));
#6964=CARTESIAN_POINT('',(-1.4,2.,4.));
#6965=CARTESIAN_POINT('',(-1.4,2.,4.));
#6966=CARTESIAN_POINT('',(-1.4,2.,8.5));
#6967=CARTESIAN_POINT('',(-1.4,2.,8.9));
#6968=CARTESIAN_POINT('',(-4.,2.,8.5));
#6969=CARTESIAN_POINT('',(2.,2.,8.5));
#6970=CARTESIAN_POINT('',(-4.,2.,9.3));
#6971=CARTESIAN_POINT('',(-4.,2.,8.5));
#6972=CARTESIAN_POINT('',(2.,2.,9.3));
#6973=CARTESIAN_POINT('',(2.,2.,9.3));
#6974=CARTESIAN_POINT('',(2.,2.,8.5));
#6975=CARTESIAN_POINT('',(2.,2.,8.5));
#6976=CARTESIAN_POINT('',(1.4,2.,8.5));
#6977=CARTESIAN_POINT('',(2.,2.,8.5));
#6978=CARTESIAN_POINT('',(1.4,2.,4.));
#6979=CARTESIAN_POINT('',(1.4,2.,4.));
#6980=CARTESIAN_POINT('',(-1.4,2.,4.));
#6981=CARTESIAN_POINT('Origin',(1.4,1.5,4.));
#6982=CARTESIAN_POINT('',(-1.4,1.5,4.));
#6983=CARTESIAN_POINT('',(-1.4,1.5,4.));
#6984=CARTESIAN_POINT('',(-1.4,1.5,4.));
#6985=CARTESIAN_POINT('Origin',(1.4,1.5,4.));
#6986=CARTESIAN_POINT('',(1.4,1.5,4.));
#6987=CARTESIAN_POINT('',(1.4,1.5,4.));
#6988=CARTESIAN_POINT('',(-1.4,1.5,4.));
#6989=CARTESIAN_POINT('Origin',(-4.,-2.,8.5));
#6990=CARTESIAN_POINT('',(1.4,-2.,4.));
#6991=CARTESIAN_POINT('',(-1.4,-2.,4.));
#6992=CARTESIAN_POINT('',(1.4,-2.,8.5));
#6993=CARTESIAN_POINT('',(1.4,-2.,4.));
#6994=CARTESIAN_POINT('',(2.,-2.,8.5));
#6995=CARTESIAN_POINT('',(-4.,-2.,8.5));
#6996=CARTESIAN_POINT('',(2.,-2.,9.3));
#6997=CARTESIAN_POINT('',(2.,-2.,8.5));
#6998=CARTESIAN_POINT('',(-4.,-2.,9.3));
#6999=CARTESIAN_POINT('',(-4.,-2.,9.3));
#7000=CARTESIAN_POINT('',(-4.,-2.,8.5));
#7001=CARTESIAN_POINT('',(-4.,-2.,8.5));
#7002=CARTESIAN_POINT('',(-1.4,-2.,8.5));
#7003=CARTESIAN_POINT('',(-4.,-2.,8.5));
#7004=CARTESIAN_POINT('',(-1.4,-2.,4.));
#7005=CARTESIAN_POINT('',(-1.4,-2.,8.9));
#7006=CARTESIAN_POINT('',(-1.4,-2.,4.));
#7007=CARTESIAN_POINT('Origin',(1.4,-2.,4.));
#7008=CARTESIAN_POINT('',(1.4,-1.5,4.));
#7009=CARTESIAN_POINT('',(-1.4,-1.5,4.));
#7010=CARTESIAN_POINT('',(1.4,-2.,4.));
#7011=CARTESIAN_POINT('Origin',(-1.4,1.5,4.));
#7012=CARTESIAN_POINT('',(-1.4,1.5,8.5));
#7013=CARTESIAN_POINT('',(-1.4,0.75,8.5));
#7014=CARTESIAN_POINT('',(-1.4,1.5,8.9));
#7015=CARTESIAN_POINT('Origin',(1.4,1.5,8.9));
#7016=CARTESIAN_POINT('',(1.4,1.5,8.5));
#7017=CARTESIAN_POINT('',(1.4,0.75,8.5));
#7018=CARTESIAN_POINT('',(1.4,1.5,4.));
#7019=CARTESIAN_POINT('Origin',(0.,1.5,6.45));
#7020=CARTESIAN_POINT('',(-0.5,1.5,8.5));
#7021=CARTESIAN_POINT('Origin',(-1.,0.,8.5));
#7022=CARTESIAN_POINT('',(2.,-2.,8.5));
#7023=CARTESIAN_POINT('',(1.4,-1.5,8.5));
#7024=CARTESIAN_POINT('',(1.4,-1.,8.5));
#7025=CARTESIAN_POINT('',(-1.4,-1.5,8.5));
#7026=CARTESIAN_POINT('',(-0.5,-1.5,8.5));
#7027=CARTESIAN_POINT('',(-1.4,-1.,8.5));
#7028=CARTESIAN_POINT('',(-4.,2.,8.5));
#7029=CARTESIAN_POINT('Origin',(0.,-1.5,6.45));
#7030=CARTESIAN_POINT('',(-1.4,-1.5,4.));
#7031=CARTESIAN_POINT('',(-1.4,-1.5,4.));
#7032=CARTESIAN_POINT('',(-1.4,-1.5,8.9));
#7033=CARTESIAN_POINT('',(1.4,-1.5,4.));
#7034=CARTESIAN_POINT('Origin',(1.4,-2.,8.9));
#7035=CARTESIAN_POINT('Origin',(-1.4,-2.,4.));
#7036=CARTESIAN_POINT('',(-1.4,-2.,4.));
#7037=CARTESIAN_POINT('Origin',(1.4,-2.,4.));
#7038=CARTESIAN_POINT('Origin',(2.,-2.,8.5));
#7039=CARTESIAN_POINT('',(2.,-2.,9.3));
#7040=CARTESIAN_POINT('Origin',(-4.,2.,8.5));
#7041=CARTESIAN_POINT('',(-4.,2.,9.3));
#7042=CARTESIAN_POINT('Origin',(-1.,0.,9.3));
#7043=CARTESIAN_POINT('',(0.,0.,0.));
#7044=CARTESIAN_POINT('Origin',(-2.,0.,8.5));
#7045=CARTESIAN_POINT('',(-2.605,-7.40911313484149E-17,9.3));
#7046=CARTESIAN_POINT('Origin',(-2.,0.,9.3));
#7047=CARTESIAN_POINT('',(-2.605,-7.40911313484149E-17,8.5));
#7048=CARTESIAN_POINT('',(-2.605,-7.40911313484149E-17,8.5));
#7049=CARTESIAN_POINT('Origin',(-2.,0.,8.5));
#7050=CARTESIAN_POINT('Origin',(-2.,0.,8.5));
#7051=CARTESIAN_POINT('',(-2.8,-9.79717439317883E-17,9.3));
#7052=CARTESIAN_POINT('Origin',(-2.,0.,9.3));
#7053=CARTESIAN_POINT('',(-2.8,-9.79717439317883E-17,8.5));
#7054=CARTESIAN_POINT('',(-2.8,-9.79717439317883E-17,8.5));
#7055=CARTESIAN_POINT('Origin',(-2.,0.,8.5));
#7056=CARTESIAN_POINT('Origin',(-2.,0.,9.3));
#7057=CARTESIAN_POINT('Origin',(-2.,0.,8.5));
#7058=CARTESIAN_POINT('',(0.,0.,0.));
#7059=CARTESIAN_POINT('Origin',(0.,0.9,3.5));
#7060=CARTESIAN_POINT('',(-0.165,0.9,3.5));
#7061=CARTESIAN_POINT('Origin',(0.,0.9,3.5));
#7062=CARTESIAN_POINT('',(-0.165,2.,3.5));
#7063=CARTESIAN_POINT('',(-0.165,0.9,3.5));
#7064=CARTESIAN_POINT('Origin',(0.,2.,3.5));
#7065=CARTESIAN_POINT('Origin',(0.,0.9,3.5));
#7066=CARTESIAN_POINT('Origin',(0.,-2.,3.5));
#7067=CARTESIAN_POINT('',(-0.9,-2.,3.5));
#7068=CARTESIAN_POINT('Origin',(0.,-2.,3.5));
#7069=CARTESIAN_POINT('',(-0.6,-2.,3.5));
#7070=CARTESIAN_POINT('Origin',(0.,-2.,3.5));
#7071=CARTESIAN_POINT('Origin',(0.,-2.4,3.5));
#7072=CARTESIAN_POINT('',(-0.9,-2.4,3.5));
#7073=CARTESIAN_POINT('',(-0.9,-2.4,3.5));
#7074=CARTESIAN_POINT('Origin',(0.,-2.4,3.5));
#7075=CARTESIAN_POINT('Origin',(0.,-2.4,3.5));
#7076=CARTESIAN_POINT('Origin',(0.,-2.,3.5));
#7077=CARTESIAN_POINT('',(-0.6,2.,3.5));
#7078=CARTESIAN_POINT('Origin',(0.,2.,3.5));
#7079=CARTESIAN_POINT('',(-0.6,-2.,3.5));
#7080=CARTESIAN_POINT('Origin',(0.,2.,3.5));
#7081=CARTESIAN_POINT('',(0.,0.,0.));
#7082=CARTESIAN_POINT('Origin',(0.,4.5,10.));
#7083=CARTESIAN_POINT('',(-0.605,4.9,10.));
#7084=CARTESIAN_POINT('Origin',(0.,4.9,10.));
#7085=CARTESIAN_POINT('',(-0.605,4.5,10.));
#7086=CARTESIAN_POINT('',(-0.605,4.5,10.));
#7087=CARTESIAN_POINT('Origin',(0.,4.5,10.));
#7088=CARTESIAN_POINT('Origin',(0.,4.5,10.));
#7089=CARTESIAN_POINT('',(-0.8,4.9,10.));
#7090=CARTESIAN_POINT('Origin',(0.,4.9,10.));
#7091=CARTESIAN_POINT('',(-0.8,4.5,10.));
#7092=CARTESIAN_POINT('',(-0.8,4.5,10.));
#7093=CARTESIAN_POINT('Origin',(0.,4.5,10.));
#7094=CARTESIAN_POINT('Origin',(0.,4.9,10.));
#7095=CARTESIAN_POINT('Origin',(0.,4.5,10.));
#7096=CARTESIAN_POINT('',(0.,0.,0.));
#7097=CARTESIAN_POINT('Origin',(0.,2.2,4.));
#7098=CARTESIAN_POINT('',(-0.225,2.4,4.));
#7099=CARTESIAN_POINT('Origin',(0.,2.4,4.));
#7100=CARTESIAN_POINT('',(-0.225,2.2,4.));
#7101=CARTESIAN_POINT('',(-0.225,2.2,4.));
#7102=CARTESIAN_POINT('Origin',(0.,2.2,4.));
#7103=CARTESIAN_POINT('Origin',(0.,2.2,4.));
#7104=CARTESIAN_POINT('',(-0.8,2.4,4.));
#7105=CARTESIAN_POINT('Origin',(0.,2.4,4.));
#7106=CARTESIAN_POINT('',(-0.8,2.2,4.));
#7107=CARTESIAN_POINT('',(-0.8,2.2,4.));
#7108=CARTESIAN_POINT('Origin',(0.,2.2,4.));
#7109=CARTESIAN_POINT('Origin',(0.,2.4,4.));
#7110=CARTESIAN_POINT('Origin',(0.,2.2,4.));
#7111=CARTESIAN_POINT('',(0.,0.,0.));
#7112=CARTESIAN_POINT('Origin',(0.0866025403784439,-0.4,-0.15));
#7113=CARTESIAN_POINT('',(0.173205080756888,-0.4,0.));
#7114=CARTESIAN_POINT('',(0.0866025403784439,-0.4,-0.15));
#7115=CARTESIAN_POINT('',(0.173205080756888,-0.4,0.));
#7116=CARTESIAN_POINT('',(0.0866025403784439,-0.64,-0.15));
#7117=CARTESIAN_POINT('',(0.0866025403784439,-0.4,-0.15));
#7118=CARTESIAN_POINT('',(0.173205080756888,-0.64,0.));
#7119=CARTESIAN_POINT('',(0.173205080756888,-0.64,0.));
#7120=CARTESIAN_POINT('',(0.173205080756888,-0.4,0.));
#7121=CARTESIAN_POINT('Origin',(-0.0866025403784438,-0.4,-0.15));
#7122=CARTESIAN_POINT('',(-0.0866025403784438,-0.4,-0.15));
#7123=CARTESIAN_POINT('',(0.0866025403784439,-0.4,-0.15));
#7124=CARTESIAN_POINT('',(-0.0866025403784438,-0.64,-0.15));
#7125=CARTESIAN_POINT('',(-0.0866025403784438,-0.4,-0.15));
#7126=CARTESIAN_POINT('',(0.0866025403784439,-0.64,-0.15));
#7127=CARTESIAN_POINT('Origin',(-0.173205080756888,-0.4,-2.77555756156289E-17));
#7128=CARTESIAN_POINT('',(-0.173205080756888,-0.4,-2.12115047744981E-17));
#7129=CARTESIAN_POINT('',(-0.0866025403784438,-0.4,-0.15));
#7130=CARTESIAN_POINT('',(-0.173205080756888,-0.64,-2.77555756156289E-17));
#7131=CARTESIAN_POINT('',(-0.173205080756888,-0.4,-2.12115047744981E-17));
#7132=CARTESIAN_POINT('',(-0.0866025403784438,-0.64,-0.15));
#7133=CARTESIAN_POINT('Origin',(-0.0866025403784439,-0.4,0.15));
#7134=CARTESIAN_POINT('',(-0.0866025403784439,-0.4,0.15));
#7135=CARTESIAN_POINT('',(-0.173205080756888,-0.4,-2.12115047744981E-17));
#7136=CARTESIAN_POINT('',(-0.0866025403784439,-0.64,0.15));
#7137=CARTESIAN_POINT('',(-0.0866025403784439,-0.4,0.15));
#7138=CARTESIAN_POINT('',(-0.173205080756888,-0.64,-2.12115047744981E-17));
#7139=CARTESIAN_POINT('Origin',(0.0866025403784439,-0.4,0.15));
#7140=CARTESIAN_POINT('',(0.0866025403784439,-0.4,0.15));
#7141=CARTESIAN_POINT('',(-0.0866025403784439,-0.4,0.15));
#7142=CARTESIAN_POINT('',(0.0866025403784439,-0.64,0.15));
#7143=CARTESIAN_POINT('',(0.0866025403784439,-0.4,0.15));
#7144=CARTESIAN_POINT('',(-0.0866025403784439,-0.64,0.15));
#7145=CARTESIAN_POINT('Origin',(0.173205080756888,-0.4,0.));
#7146=CARTESIAN_POINT('',(0.0866025403784439,-0.4,0.15));
#7147=CARTESIAN_POINT('',(0.0866025403784439,-0.64,0.15));
#7148=CARTESIAN_POINT('Origin',(0.,-0.4,-2.77555756156289E-17));
#7149=CARTESIAN_POINT('Origin',(0.,-0.64,-2.77555756156289E-17));
#7150=CARTESIAN_POINT('Origin',(0.,-1.,0.));
#7151=CARTESIAN_POINT('',(-0.1954,-1.,2.39295984553393E-17));
#7152=CARTESIAN_POINT('Origin',(0.,-1.,0.));
#7153=CARTESIAN_POINT('Origin',(0.3,0.4,0.));
#7154=CARTESIAN_POINT('',(-0.3,0.4,-3.67394039744206E-17));
#7155=CARTESIAN_POINT('Origin',(0.,0.4,0.));
#7156=CARTESIAN_POINT('Origin',(0.,0.375,0.));
#7157=CARTESIAN_POINT('',(-0.35,0.35,-4.28626379701573E-17));
#7158=CARTESIAN_POINT('Origin',(0.,0.35,0.));
#7159=CARTESIAN_POINT('',(-0.325,0.375,-3.9801020972289E-17));
#7160=CARTESIAN_POINT('Origin',(0.,0.19,0.));
#7161=CARTESIAN_POINT('',(-0.35,0.03,-4.28626379701574E-17));
#7162=CARTESIAN_POINT('Origin',(0.,0.03,0.));
#7163=CARTESIAN_POINT('',(-0.35,0.19,-4.28626379701574E-17));
#7164=CARTESIAN_POINT('Origin',(0.,0.0149999999999999,0.));
#7165=CARTESIAN_POINT('',(-0.32,-3.29597460435593E-17,-3.91886975727153E-17));
#7166=CARTESIAN_POINT('Origin',(0.,0.,0.));
#7167=CARTESIAN_POINT('',(-0.335,0.0149999999999999,-4.10256677714363E-17));
#7168=CARTESIAN_POINT('Origin',(0.22,0.,0.));
#7169=CARTESIAN_POINT('',(-0.22,-6.93889390390723E-18,-2.69422295812418E-17));
#7170=CARTESIAN_POINT('Origin',(0.,0.,0.));
#7171=CARTESIAN_POINT('Origin',(0.,-0.02,0.));
#7172=CARTESIAN_POINT('',(-0.1954,-0.0492,2.39295984553393E-17));
#7173=CARTESIAN_POINT('Origin',(0.,-0.0492,0.));
#7174=CARTESIAN_POINT('',(-0.21,-0.02,-2.57175827820944E-17));
#7175=CARTESIAN_POINT('Origin',(0.,-0.8,0.));
#7176=CARTESIAN_POINT('',(-0.1954,-0.8,-2.39295984553393E-17));
#7177=CARTESIAN_POINT('',(0.,0.,0.));
#7178=CARTESIAN_POINT('',(0.,0.,0.));
#7179=CARTESIAN_POINT('',(0.,0.,0.5));
#7180=CARTESIAN_POINT('',(0.,-3.4,-6.));
#7181=CARTESIAN_POINT('',(0.,-6.,-6.));
#7182=CARTESIAN_POINT('',(0.,-0.2,0.));
#7183=CARTESIAN_POINT('',(0.,2.2,4.));
#7184=CARTESIAN_POINT('',(0.,0.,0.));
#7185=CARTESIAN_POINT('',(0.,0.,0.));
#7186=CARTESIAN_POINT('Origin',(0.,0.1,4.));
#7187=CARTESIAN_POINT('',(-1.6,0.1,4.));
#7188=CARTESIAN_POINT('Origin',(0.,0.1,4.));
#7189=CARTESIAN_POINT('',(-1.6,1.2,4.));
#7190=CARTESIAN_POINT('',(-1.6,0.1,4.));
#7191=CARTESIAN_POINT('Origin',(0.,1.2,4.));
#7192=CARTESIAN_POINT('Origin',(0.,0.1,4.));
#7193=CARTESIAN_POINT('',(-0.62,0.1,4.));
#7194=CARTESIAN_POINT('Origin',(0.,0.1,4.));
#7195=CARTESIAN_POINT('Origin',(0.,-1.3,4.));
#7196=CARTESIAN_POINT('',(-1.6,-1.2,4.));
#7197=CARTESIAN_POINT('Origin',(0.,-1.2,4.));
#7198=CARTESIAN_POINT('',(-1.6,-0.0999999999999999,4.));
#7199=CARTESIAN_POINT('',(-1.6,-1.3,4.));
#7200=CARTESIAN_POINT('Origin',(0.,-0.0999999999999999,4.));
#7201=CARTESIAN_POINT('Origin',(0.,-0.0999999999999999,4.));
#7202=CARTESIAN_POINT('',(-0.62,-0.0999999999999999,4.));
#7203=CARTESIAN_POINT('Origin',(0.,-0.0999999999999999,4.));
#7204=CARTESIAN_POINT('Origin',(0.,-1.3,4.));
#7205=CARTESIAN_POINT('',(-0.62,-1.3,4.));
#7206=CARTESIAN_POINT('Origin',(0.,-1.2,4.));
#7207=CARTESIAN_POINT('',(-3.75,1.2,4.));
#7208=CARTESIAN_POINT('Origin',(0.,1.2,4.));
#7209=CARTESIAN_POINT('',(-3.75,-1.2,4.));
#7210=CARTESIAN_POINT('',(-3.75,-1.2,4.));
#7211=CARTESIAN_POINT('Origin',(0.,-1.2,4.));
#7212=CARTESIAN_POINT('Origin',(0.,1.2,4.));
#7213=CARTESIAN_POINT('Origin',(0.,-1.2,4.));
#7214=CARTESIAN_POINT('',(0.,0.,0.));
#7215=CARTESIAN_POINT('',(0.,0.,0.));
#7216=CARTESIAN_POINT('Origin',(0.,0.,0.));
#7217=CARTESIAN_POINT('',(-1.070235,-0.308121667383195,-1.31065986708547E-16));
#7218=CARTESIAN_POINT('',(-1.31065986708547E-16,-0.308121667383195,1.070235));
#7219=CARTESIAN_POINT('Origin',(0.,-0.308121667383195,0.));
#7220=CARTESIAN_POINT('Origin',(0.,-0.308121667383195,0.));
#7221=CARTESIAN_POINT('',(-1.31065986708547E-16,0.308121667383195,1.070235));
#7222=CARTESIAN_POINT('Origin',(-1.34711147906209E-16,0.,1.1));
#7223=CARTESIAN_POINT('',(-1.070235,0.308121667383195,1.31065986708547E-16));
#7224=CARTESIAN_POINT('Origin',(0.,0.308121667383195,0.));
#7225=CARTESIAN_POINT('Origin',(0.,0.308121667383195,0.));
#7226=CARTESIAN_POINT('Origin',(0.,0.,0.));
#7227=CARTESIAN_POINT('',(-1.070235,0.5,-1.31065986708547E-16));
#7228=CARTESIAN_POINT('',(-1.070235,0.,-1.31065986708547E-16));
#7229=CARTESIAN_POINT('Origin',(0.,0.5,0.));
#7230=CARTESIAN_POINT('Origin',(0.,0.,0.));
#7231=CARTESIAN_POINT('',(-0.6,-0.44,-7.34788079488412E-17));
#7232=CARTESIAN_POINT('Origin',(0.,-0.44,0.));
#7233=CARTESIAN_POINT('',(-0.6,0.44,-7.34788079488412E-17));
#7234=CARTESIAN_POINT('',(-0.6,0.,-7.34788079488412E-17));
#7235=CARTESIAN_POINT('Origin',(0.,0.44,0.));
#7236=CARTESIAN_POINT('Origin',(0.,0.47,0.));
#7237=CARTESIAN_POINT('',(-0.66,0.5,-8.08266887437253E-17));
#7238=CARTESIAN_POINT('',(-0.63,0.47,-7.71527483462832E-17));
#7239=CARTESIAN_POINT('Origin',(0.,0.5,0.));
#7240=CARTESIAN_POINT('Origin',(1.070235,0.5,0.));
#7241=CARTESIAN_POINT('Origin',(0.,0.,0.));
#7242=CARTESIAN_POINT('',(-1.070235,-0.5,-1.31065986708547E-16));
#7243=CARTESIAN_POINT('Origin',(0.,-0.5,0.));
#7244=CARTESIAN_POINT('',(-1.070235,0.,-1.31065986708547E-16));
#7245=CARTESIAN_POINT('Origin',(0.66,-0.5,0.));
#7246=CARTESIAN_POINT('',(-0.66,-0.5,-8.08266887437253E-17));
#7247=CARTESIAN_POINT('Origin',(0.,-0.5,0.));
#7248=CARTESIAN_POINT('Origin',(0.,-0.47,0.));
#7249=CARTESIAN_POINT('',(-0.63,-0.47,-7.71527483462832E-17));
#7250=CARTESIAN_POINT('',(0.,0.,0.));
#7251=CARTESIAN_POINT('Origin',(0.,0.,0.));
#7252=CARTESIAN_POINT('',(-1.129765,0.308121667383195,-1.38356309103871E-16));
#7253=CARTESIAN_POINT('',(-1.38356309103871E-16,0.308121667383195,1.129765));
#7254=CARTESIAN_POINT('Origin',(0.,0.308121667383195,0.));
#7255=CARTESIAN_POINT('Origin',(0.,0.308121667383195,0.));
#7256=CARTESIAN_POINT('',(-1.38356309103871E-16,-0.308121667383195,1.129765));
#7257=CARTESIAN_POINT('Origin',(-1.34711147906209E-16,0.,1.1));
#7258=CARTESIAN_POINT('',(-1.129765,-0.308121667383195,1.38356309103871E-16));
#7259=CARTESIAN_POINT('Origin',(0.,-0.308121667383195,0.));
#7260=CARTESIAN_POINT('Origin',(0.,-0.308121667383195,0.));
#7261=CARTESIAN_POINT('Origin',(0.,0.,0.));
#7262=CARTESIAN_POINT('',(-1.129765,-0.5,-1.38356309103871E-16));
#7263=CARTESIAN_POINT('Origin',(0.,-0.5,0.));
#7264=CARTESIAN_POINT('',(-1.129765,0.,-1.38356309103871E-16));
#7265=CARTESIAN_POINT('Origin',(1.54,0.5,0.));
#7266=CARTESIAN_POINT('',(-1.54,0.5,-1.88595607068692E-16));
#7267=CARTESIAN_POINT('Origin',(0.,0.5,0.));
#7268=CARTESIAN_POINT('',(-1.129765,0.5,-1.38356309103871E-16));
#7269=CARTESIAN_POINT('Origin',(0.,0.5,0.));
#7270=CARTESIAN_POINT('Origin',(0.,0.47,0.));
#7271=CARTESIAN_POINT('',(-1.6,0.44,-1.95943487863577E-16));
#7272=CARTESIAN_POINT('Origin',(0.,0.44,0.));
#7273=CARTESIAN_POINT('',(-1.57,0.47,-1.92269547466134E-16));
#7274=CARTESIAN_POINT('Origin',(0.,0.,0.));
#7275=CARTESIAN_POINT('',(-1.6,-0.44,-1.95943487863577E-16));
#7276=CARTESIAN_POINT('Origin',(0.,-0.44,0.));
#7277=CARTESIAN_POINT('',(-1.6,0.,-1.95943487863577E-16));
#7278=CARTESIAN_POINT('Origin',(0.,-0.47,0.));
#7279=CARTESIAN_POINT('',(-1.54,-0.5,-1.88595607068692E-16));
#7280=CARTESIAN_POINT('Origin',(0.,-0.5,0.));
#7281=CARTESIAN_POINT('',(-1.57,-0.47,-1.92269547466134E-16));
#7282=CARTESIAN_POINT('Origin',(1.129765,-0.5,0.));
#7283=CARTESIAN_POINT('Origin',(0.,0.,0.));
#7284=CARTESIAN_POINT('',(-1.129765,0.,-1.38356309103871E-16));
#7285=CARTESIAN_POINT('',(0.,0.,0.));
#7286=CARTESIAN_POINT('Origin',(1.1,0.,0.));
#7287=CARTESIAN_POINT('',(1.1,-2.23201749654651E-33,0.29765));
#7288=CARTESIAN_POINT('',(1.1,-2.23201749654651E-33,-0.29765));
#7289=CARTESIAN_POINT('Origin',(1.1,0.,0.));
#7290=CARTESIAN_POINT('Origin',(0.685838782044607,0.,-0.860014630714833));
#7291=CARTESIAN_POINT('',(0.918550922801216,-5.31350540756609E-33,-0.674432891191581));
#7292=CARTESIAN_POINT('',(0.453126641287998,8.49470414473068E-34,-1.04559637023808));
#7293=CARTESIAN_POINT('Origin',(0.685838782044607,0.,-0.860014630714833));
#7294=CARTESIAN_POINT('Origin',(-0.244773027351946,0.,-1.07242070340001));
#7295=CARTESIAN_POINT('',(0.0454142657089739,-2.23201749654651E-33,-1.1386540593921));
#7296=CARTESIAN_POINT('',(-0.534960320412865,-2.23201749654651E-33,-1.00618734740791));
#7297=CARTESIAN_POINT('Origin',(-0.244773027351946,0.,-1.07242070340001));
#7298=CARTESIAN_POINT('Origin',(-0.991065754692661,0.,-0.477272113029314));
#7299=CARTESIAN_POINT('',(-0.86192025974432,8.49470414473067E-34,-0.745445496560469));
#7300=CARTESIAN_POINT('',(-1.120211249641,-5.31350540756609E-33,-0.209098729498159));
#7301=CARTESIAN_POINT('Origin',(-0.991065754692661,0.,-0.477272113029314));
#7302=CARTESIAN_POINT('Origin',(-0.991065754692661,0.,0.477272113029314));
#7303=CARTESIAN_POINT('',(-1.120211249641,-2.23201749654651E-33,0.209098729498159));
#7304=CARTESIAN_POINT('',(-0.86192025974432,-2.23201749654651E-33,0.745445496560469));
#7305=CARTESIAN_POINT('Origin',(-0.991065754692661,0.,0.477272113029314));
#7306=CARTESIAN_POINT('Origin',(-0.244773027351946,0.,1.07242070340001));
#7307=CARTESIAN_POINT('',(-0.534960320412866,-2.23201749654651E-33,1.00618734740791));
#7308=CARTESIAN_POINT('',(0.0454142657089737,-2.23201749654651E-33,1.1386540593921));
#7309=CARTESIAN_POINT('Origin',(-0.244773027351946,0.,1.07242070340001));
#7310=CARTESIAN_POINT('Origin',(0.685838782044607,0.,0.860014630714833));
#7311=CARTESIAN_POINT('',(0.453126641287998,-2.23201749654651E-33,1.04559637023808));
#7312=CARTESIAN_POINT('',(0.918550922801216,-2.23201749654651E-33,0.674432891191581));
#7313=CARTESIAN_POINT('Origin',(0.685838782044607,0.,0.860014630714833));
#7314=CARTESIAN_POINT('',(0.,0.,0.));
#7315=CARTESIAN_POINT('Origin',(0.685838782044607,0.,0.860014630714833));
#7316=CARTESIAN_POINT('',(0.413083465285518,-0.05953,0.993751811093549));
#7317=CARTESIAN_POINT('',(0.876916659919095,-0.05953,0.623857181492959));
#7318=CARTESIAN_POINT('Ctrl Pts',(0.413083465285518,-0.05953,0.993751811093549));
#7319=CARTESIAN_POINT('Ctrl Pts',(0.419070565453383,-0.0925528133349865,
0.991263089003441));
#7320=CARTESIAN_POINT('Ctrl Pts',(0.430199341854858,-0.124911173756694,
0.986608710139579));
#7321=CARTESIAN_POINT('Ctrl Pts',(0.457978755888596,-0.177924977804098,
0.973971221090534));
#7322=CARTESIAN_POINT('Ctrl Pts',(0.473077587363685,-0.199697230012983,
0.966820759530997));
#7323=CARTESIAN_POINT('Ctrl Pts',(0.507057380724533,-0.237895043532788,
0.949440676105255));
#7324=CARTESIAN_POINT('Ctrl Pts',(0.525933334162555,-0.254319232363049,
0.939198248544428));
#7325=CARTESIAN_POINT('Ctrl Pts',(0.564362943424238,-0.28018331644634,0.916597376014514));
#7326=CARTESIAN_POINT('Ctrl Pts',(0.585840553788742,-0.29104845371857,0.903141581680914));
#7327=CARTESIAN_POINT('Ctrl Pts',(0.629305439856167,-0.30527573347708,0.873412008702649));
#7328=CARTESIAN_POINT('Ctrl Pts',(0.651278921914856,-0.308638795020976,
0.857118508332695));
#7329=CARTESIAN_POINT('Ctrl Pts',(0.690705563850638,-0.308638795020976,
0.825676810575914));
#7330=CARTESIAN_POINT('Ctrl Pts',(0.711480111898423,-0.30527573347708,0.807879894508811));
#7331=CARTESIAN_POINT('Ctrl Pts',(0.750136149454208,-0.29104845371857,0.772120216227122));
#7332=CARTESIAN_POINT('Ctrl Pts',(0.768033796848072,-0.28018331644634,0.754175290318038));
#7333=CARTESIAN_POINT('Ctrl Pts',(0.798619410861634,-0.254319232363049,
0.721738358858166));
#7334=CARTESIAN_POINT('Ctrl Pts',(0.812805334167529,-0.237895043532788,
0.705614819529209));
#7335=CARTESIAN_POINT('Ctrl Pts',(0.837310877969633,-0.199697230012983,
0.676354402927683));
#7336=CARTESIAN_POINT('Ctrl Pts',(0.847641868610495,-0.177924977804098,
0.663225258065736));
#7337=CARTESIAN_POINT('Ctrl Pts',(0.866144010579847,-0.124911173756694,
0.638954437806245));
#7338=CARTESIAN_POINT('Ctrl Pts',(0.873158080166742,-0.0925528133349865,
0.62914037979579));
#7339=CARTESIAN_POINT('Ctrl Pts',(0.876916659919095,-0.05953,0.623857181492959));
#7340=CARTESIAN_POINT('',(0.437601487681057,-0.05953,1.03511272300331));
#7341=CARTESIAN_POINT('Origin',(0.685838782044607,-0.05953,0.860014630714833));
#7342=CARTESIAN_POINT('',(0.911784794170997,-0.05953,0.656964154625313));
#7343=CARTESIAN_POINT('Ctrl Pts',(0.911784794170998,-0.0595300000000001,
0.656964154625312));
#7344=CARTESIAN_POINT('Ctrl Pts',(0.909827729890942,-0.0762225747374255,
0.659680317203144));
#7345=CARTESIAN_POINT('Ctrl Pts',(0.907004864562642,-0.0928409665394228,
0.663576540841106));
#7346=CARTESIAN_POINT('Ctrl Pts',(0.895234408667242,-0.144299303100741,
0.679480524217551));
#7347=CARTESIAN_POINT('Ctrl Pts',(0.882797231409153,-0.177024326825049,
0.695831250979106));
#7348=CARTESIAN_POINT('Ctrl Pts',(0.854332839576145,-0.227269801620064,
0.73042219438957));
#7349=CARTESIAN_POINT('Ctrl Pts',(0.834863020612702,-0.251265615809407,
0.752807465209441));
#7350=CARTESIAN_POINT('Ctrl Pts',(0.800439809856111,-0.279889827963178,
0.789147407129766));
#7351=CARTESIAN_POINT('Ctrl Pts',(0.781998747691871,-0.290879136862659,
0.80756613568454));
#7352=CARTESIAN_POINT('Ctrl Pts',(0.742239891936898,-0.305251990234487,
0.844254137480382));
#7353=CARTESIAN_POINT('Ctrl Pts',(0.720906778729541,-0.308638795020976,
0.862505527716294));
#7354=CARTESIAN_POINT('Ctrl Pts',(0.680463863683392,-0.308638795020976,
0.894757676234429));
#7355=CARTESIAN_POINT('Ctrl Pts',(0.657923009631182,-0.305251990234488,
0.91149460735272));
#7356=CARTESIAN_POINT('Ctrl Pts',(0.613307674922609,-0.290879136862659,
0.942092777160053));
#7357=CARTESIAN_POINT('Ctrl Pts',(0.591247219971725,-0.279889827963178,
0.955972930713954));
#7358=CARTESIAN_POINT('Ctrl Pts',(0.548158511259202,-0.251265615809407,
0.981446681891443));
#7359=CARTESIAN_POINT('Ctrl Pts',(0.522002043615455,-0.227269801620063,
0.995447160474328));
#7360=CARTESIAN_POINT('Ctrl Pts',(0.481944444320713,-0.177024326825049,
1.01550068154148));
#7361=CARTESIAN_POINT('Ctrl Pts',(0.463236132117164,-0.14429930310074,1.0239876538093));
#7362=CARTESIAN_POINT('Ctrl Pts',(0.445111721969657,-0.0928409665394226,
1.03192403056628));
#7363=CARTESIAN_POINT('Ctrl Pts',(0.440685038163619,-0.0762225747374254,
1.03380912944435));
#7364=CARTESIAN_POINT('Ctrl Pts',(0.437601487681056,-0.05953,1.03511272300331));
#7365=CARTESIAN_POINT('Origin',(0.685838782044607,-0.05953,0.860014630714833));
#7366=CARTESIAN_POINT('Origin',(0.,-0.208355,0.));
#7367=CARTESIAN_POINT('',(0.0548532617164168,-0.05953,1.12247250791415));
#7368=CARTESIAN_POINT('Origin',(0.,-0.05953,0.));
#7369=CARTESIAN_POINT('',(-0.536443649899848,-0.05953,0.987512846410683));
#7370=CARTESIAN_POINT('Ctrl Pts',(0.0548532617164173,-0.0595300000000001,
1.12247250791414));
#7371=CARTESIAN_POINT('Ctrl Pts',(0.05150947068137,-0.0762225747374254,
1.12263591311425));
#7372=CARTESIAN_POINT('Ctrl Pts',(0.0467032526342597,-0.0928409665394227,
1.12285816383385));
#7373=CARTESIAN_POINT('Ctrl Pts',(0.0269302585198975,-0.144299303100741,
1.12357162229597));
#7374=CARTESIAN_POINT('Ctrl Pts',(0.006392292392153,-0.177024326825049,
1.12404235695137));
#7375=CARTESIAN_POINT('Ctrl Pts',(-0.0383992541984087,-0.227269801620063,
1.12335509974011));
#7376=CARTESIAN_POINT('Ctrl Pts',(-0.0680399972366993,-0.251265615809407,
1.12208997038458));
#7377=CARTESIAN_POINT('Ctrl Pts',(-0.117914228755037,-0.279889827963178,
1.1178344036749));
#7378=CARTESIAN_POINT('Ctrl Pts',(-0.14381238480104,-0.290879136862659,
1.11490049012186));
#7379=CARTESIAN_POINT('Ctrl Pts',(-0.19728546073067,-0.305251990234488,
1.10669035995599));
#7380=CARTESIAN_POINT('Ctrl Pts',(-0.224855950742601,-0.308638795020976,
1.10139101611326));
#7381=CARTESIAN_POINT('Ctrl Pts',(-0.275287440920027,-0.308638795020976,
1.0898803575765));
#7382=CARTESIAN_POINT('Ctrl Pts',(-0.302426893214945,-0.305251990234488,
1.08269251410343));
#7383=CARTESIAN_POINT('Ctrl Pts',(-0.35416671187353,-0.290879136862659,
1.06688848765783));
#7384=CARTESIAN_POINT('Ctrl Pts',(-0.3787731215897,-0.279889827963178,1.05829506364875));
#7385=CARTESIAN_POINT('Ctrl Pts',(-0.425554672694338,-0.251265615809407,
1.04048957871266));
#7386=CARTESIAN_POINT('Ctrl Pts',(-0.452808978448581,-0.227269801620063,
1.02876878445619));
#7387=CARTESIAN_POINT('Ctrl Pts',(-0.493462957200432,-0.177024326825049,
1.0099536580922));
#7388=CARTESIAN_POINT('Ctrl Pts',(-0.511762781179148,-0.14429930310074,
1.00061845128527));
#7389=CARTESIAN_POINT('Ctrl Pts',(-0.529268075276157,-0.0928409665394226,
0.991396466802468));
#7390=CARTESIAN_POINT('Ctrl Pts',(-0.533501897135713,-0.0762225747374254,
0.989110885965947));
#7391=CARTESIAN_POINT('Ctrl Pts',(-0.536443649899848,-0.0595300000000001,
0.987512846410683));
#7392=CARTESIAN_POINT('',(-0.843383895613249,-0.05953,0.742736168477219));
#7393=CARTESIAN_POINT('Origin',(0.,-0.05953,0.));
#7394=CARTESIAN_POINT('',(-1.10653577764992,-0.05953,0.196295654879792));
#7395=CARTESIAN_POINT('Ctrl Pts',(-0.843383895613249,-0.0595300000000001,
0.742736168477219));
#7396=CARTESIAN_POINT('Ctrl Pts',(-0.84559647055299,-0.0762225747374255,
0.740223768851062));
#7397=CARTESIAN_POINT('Ctrl Pts',(-0.848766861100456,-0.0928409665394227,
0.736604687327351));
#7398=CARTESIAN_POINT('Ctrl Pts',(-0.861652925570091,-0.144299303100741,
0.721590372101268));
#7399=CARTESIAN_POINT('Ctrl Pts',(-0.87482617317514,-0.177024326825049,
0.705826641853758));
#7400=CARTESIAN_POINT('Ctrl Pts',(-0.902215926359523,-0.227269801620063,
0.670378702718353));
#7401=CARTESIAN_POINT('Ctrl Pts',(-0.919707509403859,-0.251265615809407,
0.646415841396062));
#7402=CARTESIAN_POINT('Ctrl Pts',(-0.947476448101718,-0.279889827963178,
0.604769294586516));
#7403=CARTESIAN_POINT('Ctrl Pts',(-0.961329858300736,-0.290879136862659,
0.582692035672022));
#7404=CARTESIAN_POINT('Ctrl Pts',(-0.988250837578047,-0.305251990234488,
0.535766169015486));
#7405=CARTESIAN_POINT('Ctrl Pts',(-1.00129756308006,-0.308638795020976,
0.510906605094603));
#7406=CARTESIAN_POINT('Ctrl Pts',(-1.02374168767024,-0.308638795020976,
0.46430090015576));
#7407=CARTESIAN_POINT('Ctrl Pts',(-1.03504317708586,-0.305251990234488,
0.438600874831839));
#7408=CARTESIAN_POINT('Ctrl Pts',(-1.05494634094458,-0.290879136862659,
0.388295406390235));
#7409=CARTESIAN_POINT('Ctrl Pts',(-1.06356957703048,-0.279889827963178,
0.363699428370917));
#7410=CARTESIAN_POINT('Ctrl Pts',(-1.0788165083757,-0.251265615809407,0.316022600643821));
#7411=CARTESIAN_POINT('Ctrl Pts',(-1.08664560412098,-0.227269801620063,
0.287406530683752));
#7412=CARTESIAN_POINT('Ctrl Pts',(-1.09728268713976,-0.177024326825049,
0.243890930799337));
#7413=CARTESIAN_POINT('Ctrl Pts',(-1.10139388218929,-0.144299303100741,
0.22376314604679));
#7414=CARTESIAN_POINT('Ctrl Pts',(-1.10509821673782,-0.0928409665394227,
0.204327142733961));
#7415=CARTESIAN_POINT('Ctrl Pts',(-1.10595102243643,-0.0762225747374254,
0.199591971170104));
#7416=CARTESIAN_POINT('Ctrl Pts',(-1.10653577764992,-0.0595300000000001,
0.196295654879792));
#7417=CARTESIAN_POINT('',(-1.123812,-0.05953,1.37627276864339E-16));
#7418=CARTESIAN_POINT('Origin',(0.,-0.05953,0.));
#7419=CARTESIAN_POINT('',(-1.123812,-0.35718,1.37627276864339E-16));
#7420=CARTESIAN_POINT('',(-1.123812,-0.208355,1.37627276864339E-16));
#7421=CARTESIAN_POINT('Origin',(0.,-0.35718,0.));
#7422=CARTESIAN_POINT('',(-1.10653577764992,-0.05953,-0.196295654879793));
#7423=CARTESIAN_POINT('Origin',(0.,-0.05953,0.));
#7424=CARTESIAN_POINT('',(-0.843383895613249,-0.05953,-0.742736168477219));
#7425=CARTESIAN_POINT('Ctrl Pts',(-1.10653577764992,-0.0595300000000001,
-0.196295654879792));
#7426=CARTESIAN_POINT('Ctrl Pts',(-1.10595102243643,-0.0762225747374255,
-0.199591971170104));
#7427=CARTESIAN_POINT('Ctrl Pts',(-1.10509821673782,-0.0928409665394228,
-0.204327142733962));
#7428=CARTESIAN_POINT('Ctrl Pts',(-1.10139388218929,-0.144299303100741,
-0.22376314604679));
#7429=CARTESIAN_POINT('Ctrl Pts',(-1.09728268713976,-0.177024326825049,
-0.243890930799338));
#7430=CARTESIAN_POINT('Ctrl Pts',(-1.08664560412098,-0.227269801620063,
-0.287406530683753));
#7431=CARTESIAN_POINT('Ctrl Pts',(-1.0788165083757,-0.251265615809407,-0.316022600643821));
#7432=CARTESIAN_POINT('Ctrl Pts',(-1.06356957703048,-0.279889827963178,
-0.363699428370918));
#7433=CARTESIAN_POINT('Ctrl Pts',(-1.05494634094458,-0.290879136862659,
-0.388295406390235));
#7434=CARTESIAN_POINT('Ctrl Pts',(-1.03504317708586,-0.305251990234488,
-0.438600874831839));
#7435=CARTESIAN_POINT('Ctrl Pts',(-1.02374168767024,-0.308638795020976,
-0.46430090015576));
#7436=CARTESIAN_POINT('Ctrl Pts',(-1.00129756308006,-0.308638795020976,
-0.510906605094603));
#7437=CARTESIAN_POINT('Ctrl Pts',(-0.988250837578047,-0.305251990234488,
-0.535766169015486));
#7438=CARTESIAN_POINT('Ctrl Pts',(-0.961329858300736,-0.290879136862659,
-0.582692035672022));
#7439=CARTESIAN_POINT('Ctrl Pts',(-0.947476448101718,-0.279889827963178,
-0.604769294586516));
#7440=CARTESIAN_POINT('Ctrl Pts',(-0.919707509403859,-0.251265615809407,
-0.646415841396062));
#7441=CARTESIAN_POINT('Ctrl Pts',(-0.902215926359523,-0.227269801620064,
-0.670378702718353));
#7442=CARTESIAN_POINT('Ctrl Pts',(-0.87482617317514,-0.177024326825049,
-0.705826641853758));
#7443=CARTESIAN_POINT('Ctrl Pts',(-0.861652925570091,-0.144299303100741,
-0.721590372101268));
#7444=CARTESIAN_POINT('Ctrl Pts',(-0.848766861100456,-0.0928409665394229,
-0.736604687327351));
#7445=CARTESIAN_POINT('Ctrl Pts',(-0.84559647055299,-0.0762225747374255,
-0.740223768851063));
#7446=CARTESIAN_POINT('Ctrl Pts',(-0.843383895613249,-0.0595300000000001,
-0.742736168477219));
#7447=CARTESIAN_POINT('',(-0.536443649899847,-0.05953,-0.987512846410683));
#7448=CARTESIAN_POINT('Origin',(0.,-0.05953,0.));
#7449=CARTESIAN_POINT('',(0.0548532617164172,-0.05953,-1.12247250791415));
#7450=CARTESIAN_POINT('Ctrl Pts',(-0.536443649899848,-0.0595300000000001,
-0.987512846410683));
#7451=CARTESIAN_POINT('Ctrl Pts',(-0.533501897135712,-0.0762225747374254,
-0.989110885965947));
#7452=CARTESIAN_POINT('Ctrl Pts',(-0.529268075276156,-0.0928409665394227,
-0.991396466802469));
#7453=CARTESIAN_POINT('Ctrl Pts',(-0.511762781179147,-0.144299303100741,
-1.00061845128527));
#7454=CARTESIAN_POINT('Ctrl Pts',(-0.493462957200432,-0.177024326825049,
-1.0099536580922));
#7455=CARTESIAN_POINT('Ctrl Pts',(-0.45280897844858,-0.227269801620063,
-1.02876878445619));
#7456=CARTESIAN_POINT('Ctrl Pts',(-0.425554672694337,-0.251265615809407,
-1.04048957871266));
#7457=CARTESIAN_POINT('Ctrl Pts',(-0.3787731215897,-0.279889827963178,-1.05829506364875));
#7458=CARTESIAN_POINT('Ctrl Pts',(-0.354166711873529,-0.290879136862659,
-1.06688848765783));
#7459=CARTESIAN_POINT('Ctrl Pts',(-0.302426893214944,-0.305251990234488,
-1.08269251410343));
#7460=CARTESIAN_POINT('Ctrl Pts',(-0.275287440920027,-0.308638795020976,
-1.0898803575765));
#7461=CARTESIAN_POINT('Ctrl Pts',(-0.224855950742601,-0.308638795020976,
-1.10139101611326));
#7462=CARTESIAN_POINT('Ctrl Pts',(-0.19728546073067,-0.305251990234488,
-1.10669035995599));
#7463=CARTESIAN_POINT('Ctrl Pts',(-0.143812384801039,-0.290879136862659,
-1.11490049012186));
#7464=CARTESIAN_POINT('Ctrl Pts',(-0.117914228755037,-0.279889827963178,
-1.1178344036749));
#7465=CARTESIAN_POINT('Ctrl Pts',(-0.0680399972366989,-0.251265615809407,
-1.12208997038458));
#7466=CARTESIAN_POINT('Ctrl Pts',(-0.0383992541984084,-0.227269801620063,
-1.12335509974011));
#7467=CARTESIAN_POINT('Ctrl Pts',(0.00639229239215326,-0.177024326825049,
-1.12404235695137));
#7468=CARTESIAN_POINT('Ctrl Pts',(0.0269302585198977,-0.144299303100741,
-1.12357162229597));
#7469=CARTESIAN_POINT('Ctrl Pts',(0.04670325263426,-0.0928409665394228,
-1.12285816383385));
#7470=CARTESIAN_POINT('Ctrl Pts',(0.0515094706813703,-0.0762225747374255,
-1.12263591311425));
#7471=CARTESIAN_POINT('Ctrl Pts',(0.0548532617164176,-0.0595300000000001,
-1.12247250791414));
#7472=CARTESIAN_POINT('',(0.437601487681057,-0.05953,-1.03511272300331));
#7473=CARTESIAN_POINT('Origin',(0.,-0.05953,0.));
#7474=CARTESIAN_POINT('',(0.911784794170997,-0.05953,-0.656964154625313));
#7475=CARTESIAN_POINT('Ctrl Pts',(0.437601487681056,-0.0595300000000001,
-1.03511272300331));
#7476=CARTESIAN_POINT('Ctrl Pts',(0.440685038163619,-0.0762225747374255,
-1.03380912944435));
#7477=CARTESIAN_POINT('Ctrl Pts',(0.445111721969657,-0.0928409665394228,
-1.03192403056628));
#7478=CARTESIAN_POINT('Ctrl Pts',(0.463236132117164,-0.144299303100741,
-1.0239876538093));
#7479=CARTESIAN_POINT('Ctrl Pts',(0.481944444320713,-0.177024326825049,
-1.01550068154148));
#7480=CARTESIAN_POINT('Ctrl Pts',(0.522002043615455,-0.227269801620064,
-0.995447160474328));
#7481=CARTESIAN_POINT('Ctrl Pts',(0.548158511259203,-0.251265615809407,
-0.981446681891443));
#7482=CARTESIAN_POINT('Ctrl Pts',(0.591247219971725,-0.279889827963178,
-0.955972930713954));
#7483=CARTESIAN_POINT('Ctrl Pts',(0.613307674922609,-0.290879136862659,
-0.942092777160053));
#7484=CARTESIAN_POINT('Ctrl Pts',(0.657923009631182,-0.305251990234487,
-0.91149460735272));
#7485=CARTESIAN_POINT('Ctrl Pts',(0.680463863683393,-0.308638795020976,
-0.894757676234429));
#7486=CARTESIAN_POINT('Ctrl Pts',(0.720906778729542,-0.308638795020976,
-0.862505527716294));
#7487=CARTESIAN_POINT('Ctrl Pts',(0.742239891936899,-0.305251990234488,
-0.844254137480381));
#7488=CARTESIAN_POINT('Ctrl Pts',(0.781998747691872,-0.290879136862659,
-0.80756613568454));
#7489=CARTESIAN_POINT('Ctrl Pts',(0.800439809856112,-0.279889827963178,
-0.789147407129765));
#7490=CARTESIAN_POINT('Ctrl Pts',(0.834863020612702,-0.251265615809407,
-0.752807465209441));
#7491=CARTESIAN_POINT('Ctrl Pts',(0.854332839576145,-0.227269801620064,
-0.73042219438957));
#7492=CARTESIAN_POINT('Ctrl Pts',(0.882797231409153,-0.177024326825049,
-0.695831250979106));
#7493=CARTESIAN_POINT('Ctrl Pts',(0.895234408667242,-0.144299303100741,
-0.679480524217551));
#7494=CARTESIAN_POINT('Ctrl Pts',(0.907004864562642,-0.0928409665394228,
-0.663576540841106));
#7495=CARTESIAN_POINT('Ctrl Pts',(0.909827729890942,-0.0762225747374256,
-0.659680317203144));
#7496=CARTESIAN_POINT('Ctrl Pts',(0.911784794170998,-0.0595300000000001,
-0.656964154625312));
#7497=CARTESIAN_POINT('',(1.08212377959455,-0.05953,-0.303251606722892));
#7498=CARTESIAN_POINT('Origin',(0.,-0.05953,0.));
#7499=CARTESIAN_POINT('',(1.08212377959455,-0.05953,0.303251606722892));
#7500=CARTESIAN_POINT('Ctrl Pts',(1.08212377959455,-0.0595300000000001,
-0.303251606722892));
#7501=CARTESIAN_POINT('Ctrl Pts',(1.0830271513892,-0.0762225747374255,-0.300028012588062));
#7502=CARTESIAN_POINT('Ctrl Pts',(1.08431331394788,-0.0928409665394228,
-0.2953917518996));
#7503=CARTESIAN_POINT('Ctrl Pts',(1.08940878963422,-0.144299303100741,-0.276273267473431));
#7504=CARTESIAN_POINT('Ctrl Pts',(1.09443784939331,-0.177024326825049,-0.256354979351213));
#7505=CARTESIAN_POINT('Ctrl Pts',(1.10373487993589,-0.227269801620064,-0.212533521233765));
#7506=CARTESIAN_POINT('Ctrl Pts',(1.10909715583869,-0.251265615809407,-0.183354415742157));
#7507=CARTESIAN_POINT('Ctrl Pts',(1.1160463456491,-0.279889827963178,-0.133783682657561));
#7508=CARTESIAN_POINT('Ctrl Pts',(1.11894887330541,-0.290879136862659,-0.107881990270302));
#7509=CARTESIAN_POINT('Ctrl Pts',(1.12284346704144,-0.305251990234488,-0.0539226701638766));
#7510=CARTESIAN_POINT('Ctrl Pts',(1.123812,-0.308638795020976,-0.025864214957475));
#7511=CARTESIAN_POINT('Ctrl Pts',(1.123812,-0.308638795020976,0.025864214957475));
#7512=CARTESIAN_POINT('Ctrl Pts',(1.12284346704144,-0.305251990234488,0.0539226701638766));
#7513=CARTESIAN_POINT('Ctrl Pts',(1.11894887330541,-0.290879136862659,0.107881990270302));
#7514=CARTESIAN_POINT('Ctrl Pts',(1.1160463456491,-0.279889827963178,0.133783682657561));
#7515=CARTESIAN_POINT('Ctrl Pts',(1.10909715583869,-0.251265615809407,0.183354415742157));
#7516=CARTESIAN_POINT('Ctrl Pts',(1.10373487993589,-0.227269801620064,0.212533521233765));
#7517=CARTESIAN_POINT('Ctrl Pts',(1.09443784939331,-0.177024326825049,0.256354979351213));
#7518=CARTESIAN_POINT('Ctrl Pts',(1.08940878963422,-0.144299303100741,0.276273267473431));
#7519=CARTESIAN_POINT('Ctrl Pts',(1.08431331394788,-0.0928409665394228,
0.2953917518996));
#7520=CARTESIAN_POINT('Ctrl Pts',(1.0830271513892,-0.0762225747374255,0.300028012588062));
#7521=CARTESIAN_POINT('Ctrl Pts',(1.08212377959455,-0.0595300000000001,
0.303251606722892));
#7522=CARTESIAN_POINT('Origin',(0.,-0.05953,0.));
#7523=CARTESIAN_POINT('Origin',(0.,-0.05953,0.));
#7524=CARTESIAN_POINT('',(0.0589974094846122,-0.05953,1.07456964270265));
#7525=CARTESIAN_POINT('Origin',(0.,-0.05953,0.));
#7526=CARTESIAN_POINT('Origin',(-0.244773027351946,-0.05953,1.07242070340001));
#7527=CARTESIAN_POINT('Origin',(-0.244773027351946,0.,1.07242070340001));
#7528=CARTESIAN_POINT('',(-0.519393123750572,-0.05953,0.942555777842682));
#7529=CARTESIAN_POINT('Ctrl Pts',(-0.519393123750572,-0.05953,0.942555777842682));
#7530=CARTESIAN_POINT('Ctrl Pts',(-0.513714466572041,-0.0925528133349865,
0.945684988399766));
#7531=CARTESIAN_POINT('Ctrl Pts',(-0.503136848051455,-0.124911173756694,
0.951483858396181));
#7532=CARTESIAN_POINT('Ctrl Pts',(-0.47593627990192,-0.177924977804098,
0.965323333309091));
#7533=CARTESIAN_POINT('Ctrl Pts',(-0.460931856495794,-0.199697230012983,
0.972669835243841));
#7534=CARTESIAN_POINT('Ctrl Pts',(-0.426157505475872,-0.237895043532788,
0.988400002689705));
#7535=CARTESIAN_POINT('Ctrl Pts',(-0.406380688682952,-0.254319232363049,
0.996771768218699));
#7536=CARTESIAN_POINT('Ctrl Pts',(-0.364750145543744,-0.28018331644634,
1.01272583306292));
#7537=CARTESIAN_POINT('Ctrl Pts',(-0.340838910881557,-0.29104845371857,
1.02112815447116));
#7538=CARTESIAN_POINT('Ctrl Pts',(-0.290495481564827,-0.30527573347708,
1.036574285215));
#7539=CARTESIAN_POINT('Ctrl Pts',(-0.264056468041074,-0.308638795020976,
1.04359501395068));
#7540=CARTESIAN_POINT('Ctrl Pts',(-0.214892249704082,-0.308638795020976,
1.05481642595959));
#7541=CARTESIAN_POINT('Ctrl Pts',(-0.188025341585962,-0.30527573347708,
1.05996242598502));
#7542=CARTESIAN_POINT('Ctrl Pts',(-0.135965654106109,-0.29104845371857,
1.06788913840721));
#7543=CARTESIAN_POINT('Ctrl Pts',(-0.110776745452494,-0.28018331644634,
1.07069360430242));
#7544=CARTESIAN_POINT('Ctrl Pts',(-0.0663467128214646,-0.254319232363049,
1.07438230428002));
#7545=CARTESIAN_POINT('Ctrl Pts',(-0.0448960436540983,-0.237895043532788,
1.07542044338697));
#7546=CARTESIAN_POINT('Ctrl Pts',(-0.00674037211528124,-0.199697230012983,
1.07633607767727));
#7547=CARTESIAN_POINT('Ctrl Pts',(0.00996567398334777,-0.177924977804098,
1.07622728347683));
#7548=CARTESIAN_POINT('Ctrl Pts',(0.0404772621979741,-0.124911173756694,
1.07556023164702));
#7549=CARTESIAN_POINT('Ctrl Pts',(0.0525234025782719,-0.0925528133349865,
1.07492508698591));
#7550=CARTESIAN_POINT('Ctrl Pts',(0.0589974094846124,-0.05953,1.07456964270265));
#7551=CARTESIAN_POINT('Origin',(-0.244773027351946,-0.05953,1.07242070340001));
#7552=CARTESIAN_POINT('Origin',(0.,-0.05953,0.));
#7553=CARTESIAN_POINT('',(-0.803348093619616,-0.05953,0.716109245731214));
#7554=CARTESIAN_POINT('Origin',(0.,-0.05953,0.));
#7555=CARTESIAN_POINT('Origin',(-0.991065754692661,-0.05953,0.477272113029314));
#7556=CARTESIAN_POINT('Origin',(-0.991065754692661,0.,0.477272113029314));
#7557=CARTESIAN_POINT('',(-1.06075609691358,-0.05953,0.181596019242328));
#7558=CARTESIAN_POINT('Ctrl Pts',(-1.06075609691358,-0.05953,0.181596019242328));
#7559=CARTESIAN_POINT('Ctrl Pts',(-1.05966202740332,-0.0925528133349865,
0.187986803072856));
#7560=CARTESIAN_POINT('Ctrl Pts',(-1.05760072925372,-0.124911173756694,
0.199872254546857));
#7561=CARTESIAN_POINT('Ctrl Pts',(-1.05146158959546,-0.177924977804098,
0.22976728653846));
#7562=CARTESIAN_POINT('Ctrl Pts',(-1.04785021111757,-0.199697230012983,
0.246078686169301));
#7563=CARTESIAN_POINT('Ctrl Pts',(-1.03846709802406,-0.237895043532788,
0.283073967563097));
#7564=CARTESIAN_POINT('Ctrl Pts',(-1.03268176429485,-0.254319232363049,
0.303755815985685));
#7565=CARTESIAN_POINT('Ctrl Pts',(-1.01919893537026,-0.28018331644634,0.346251081972725));
#7566=CARTESIAN_POINT('Ctrl Pts',(-1.01085972381132,-0.29104845371857,0.370184399726282));
#7567=CARTESIAN_POINT('Ctrl Pts',(-0.99154738033959,-0.30527573347708,0.419174982698463));
#7568=CARTESIAN_POINT('Ctrl Pts',(-0.980551951791748,-0.308638795020976,
0.444223188605045));
#7569=CARTESIAN_POINT('Ctrl Pts',(-0.958671816228589,-0.308638795020976,
0.489657758261848));
#7570=CARTESIAN_POINT('Ctrl Pts',(-0.945943877838127,-0.30527573347708,
0.51387163140139));
#7571=CARTESIAN_POINT('Ctrl Pts',(-0.91968254693063,-0.29104845371857,0.559515758398093));
#7572=CARTESIAN_POINT('Ctrl Pts',(-0.906170138993533,-0.28018331644634,
0.580957796077825));
#7573=CARTESIAN_POINT('Ctrl Pts',(-0.8813524085237,-0.254319232363049,0.617994461173994));
#7574=CARTESIAN_POINT('Ctrl Pts',(-0.868789784891799,-0.237895043532788,
0.635412538795143));
#7575=CARTESIAN_POINT('Ctrl Pts',(-0.845715984518854,-0.199697230012983,
0.66581473268113));
#7576=CARTESIAN_POINT('Ctrl Pts',(-0.835214876415962,-0.177924977804098,
0.678808213394124));
#7577=CARTESIAN_POINT('Ctrl Pts',(-0.815669690204649,-0.124911173756694,
0.702247233627224));
#7578=CARTESIAN_POINT('Ctrl Pts',(-0.807662468433796,-0.0925528133349865,
0.711269279199861));
#7579=CARTESIAN_POINT('Ctrl Pts',(-0.803348093619616,-0.05953,0.716109245731214));
#7580=CARTESIAN_POINT('Origin',(-0.991065754692661,-0.05953,0.477272113029314));
#7581=CARTESIAN_POINT('Origin',(0.,-0.05953,0.));
#7582=CARTESIAN_POINT('',(-1.076188,-0.05953,1.31795018948079E-16));
#7583=CARTESIAN_POINT('Origin',(0.,-0.05953,0.));
#7584=CARTESIAN_POINT('',(-1.06075609691358,-0.05953,-0.181596019242328));
#7585=CARTESIAN_POINT('Origin',(0.,-0.05953,0.));
#7586=CARTESIAN_POINT('Origin',(-0.991065754692661,-0.05953,-0.477272113029314));
#7587=CARTESIAN_POINT('Origin',(-0.991065754692661,0.,-0.477272113029314));
#7588=CARTESIAN_POINT('',(-0.803348093619616,-0.05953,-0.716109245731215));
#7589=CARTESIAN_POINT('Ctrl Pts',(-0.803348093619616,-0.05953,-0.716109245731215));
#7590=CARTESIAN_POINT('Ctrl Pts',(-0.807662468433795,-0.0925528133349865,
-0.711269279199862));
#7591=CARTESIAN_POINT('Ctrl Pts',(-0.815669690204649,-0.124911173756694,
-0.702247233627224));
#7592=CARTESIAN_POINT('Ctrl Pts',(-0.835214876415962,-0.177924977804098,
-0.678808213394124));
#7593=CARTESIAN_POINT('Ctrl Pts',(-0.845715984518854,-0.199697230012983,
-0.66581473268113));
#7594=CARTESIAN_POINT('Ctrl Pts',(-0.868789784891799,-0.237895043532788,
-0.635412538795143));
#7595=CARTESIAN_POINT('Ctrl Pts',(-0.8813524085237,-0.254319232363049,-0.617994461173994));
#7596=CARTESIAN_POINT('Ctrl Pts',(-0.906170138993533,-0.28018331644634,
-0.580957796077826));
#7597=CARTESIAN_POINT('Ctrl Pts',(-0.91968254693063,-0.29104845371857,-0.559515758398093));
#7598=CARTESIAN_POINT('Ctrl Pts',(-0.945943877838127,-0.30527573347708,
-0.51387163140139));
#7599=CARTESIAN_POINT('Ctrl Pts',(-0.958671816228589,-0.308638795020976,
-0.489657758261848));
#7600=CARTESIAN_POINT('Ctrl Pts',(-0.980551951791748,-0.308638795020976,
-0.444223188605045));
#7601=CARTESIAN_POINT('Ctrl Pts',(-0.99154738033959,-0.30527573347708,-0.419174982698463));
#7602=CARTESIAN_POINT('Ctrl Pts',(-1.01085972381132,-0.29104845371857,-0.370184399726282));
#7603=CARTESIAN_POINT('Ctrl Pts',(-1.01919893537026,-0.28018331644634,-0.346251081972725));
#7604=CARTESIAN_POINT('Ctrl Pts',(-1.03268176429485,-0.254319232363049,
-0.303755815985685));
#7605=CARTESIAN_POINT('Ctrl Pts',(-1.03846709802406,-0.237895043532788,
-0.283073967563097));
#7606=CARTESIAN_POINT('Ctrl Pts',(-1.04785021111757,-0.199697230012983,
-0.246078686169302));
#7607=CARTESIAN_POINT('Ctrl Pts',(-1.05146158959546,-0.177924977804098,
-0.229767286538461));
#7608=CARTESIAN_POINT('Ctrl Pts',(-1.05760072925372,-0.124911173756694,
-0.199872254546858));
#7609=CARTESIAN_POINT('Ctrl Pts',(-1.05966202740332,-0.0925528133349864,
-0.187986803072857));
#7610=CARTESIAN_POINT('Ctrl Pts',(-1.06075609691358,-0.05953,-0.181596019242328));
#7611=CARTESIAN_POINT('Origin',(-0.991065754692661,-0.05953,-0.477272113029314));
#7612=CARTESIAN_POINT('Origin',(0.,-0.05953,0.));
#7613=CARTESIAN_POINT('',(-0.519393123750572,-0.05953,-0.942555777842682));
#7614=CARTESIAN_POINT('Origin',(0.,-0.05953,0.));
#7615=CARTESIAN_POINT('Origin',(-0.244773027351946,-0.05953,-1.07242070340001));
#7616=CARTESIAN_POINT('Origin',(-0.244773027351946,0.,-1.07242070340001));
#7617=CARTESIAN_POINT('',(0.0589974094846125,-0.05953,-1.07456964270265));
#7618=CARTESIAN_POINT('Ctrl Pts',(0.0589974094846127,-0.05953,-1.07456964270265));
#7619=CARTESIAN_POINT('Ctrl Pts',(0.0525234025782722,-0.0925528133349865,
-1.07492508698591));
#7620=CARTESIAN_POINT('Ctrl Pts',(0.0404772621979744,-0.124911173756694,
-1.07556023164702));
#7621=CARTESIAN_POINT('Ctrl Pts',(0.0099656739833481,-0.177924977804098,
-1.07622728347683));
#7622=CARTESIAN_POINT('Ctrl Pts',(-0.00674037211528096,-0.199697230012983,
-1.07633607767727));
#7623=CARTESIAN_POINT('Ctrl Pts',(-0.044896043654098,-0.237895043532788,
-1.07542044338697));
#7624=CARTESIAN_POINT('Ctrl Pts',(-0.0663467128214644,-0.254319232363049,
-1.07438230428002));
#7625=CARTESIAN_POINT('Ctrl Pts',(-0.110776745452493,-0.28018331644634,
-1.07069360430242));
#7626=CARTESIAN_POINT('Ctrl Pts',(-0.135965654106109,-0.29104845371857,
-1.06788913840721));
#7627=CARTESIAN_POINT('Ctrl Pts',(-0.188025341585962,-0.30527573347708,
-1.05996242598502));
#7628=CARTESIAN_POINT('Ctrl Pts',(-0.214892249704082,-0.308638795020976,
-1.05481642595959));
#7629=CARTESIAN_POINT('Ctrl Pts',(-0.264056468041074,-0.308638795020976,
-1.04359501395068));
#7630=CARTESIAN_POINT('Ctrl Pts',(-0.290495481564827,-0.30527573347708,
-1.036574285215));
#7631=CARTESIAN_POINT('Ctrl Pts',(-0.340838910881557,-0.291048453718569,
-1.02112815447116));
#7632=CARTESIAN_POINT('Ctrl Pts',(-0.364750145543744,-0.28018331644634,
-1.01272583306292));
#7633=CARTESIAN_POINT('Ctrl Pts',(-0.406380688682952,-0.254319232363049,
-0.996771768218699));
#7634=CARTESIAN_POINT('Ctrl Pts',(-0.426157505475872,-0.237895043532788,
-0.988400002689705));
#7635=CARTESIAN_POINT('Ctrl Pts',(-0.460931856495794,-0.199697230012983,
-0.972669835243841));
#7636=CARTESIAN_POINT('Ctrl Pts',(-0.475936279901919,-0.177924977804098,
-0.965323333309091));
#7637=CARTESIAN_POINT('Ctrl Pts',(-0.503136848051454,-0.124911173756694,
-0.951483858396181));
#7638=CARTESIAN_POINT('Ctrl Pts',(-0.513714466572041,-0.0925528133349865,
-0.945684988399766));
#7639=CARTESIAN_POINT('Ctrl Pts',(-0.519393123750572,-0.05953,-0.942555777842682));
#7640=CARTESIAN_POINT('Origin',(-0.244773027351946,-0.05953,-1.07242070340001));
#7641=CARTESIAN_POINT('Origin',(0.,-0.05953,0.));
#7642=CARTESIAN_POINT('',(0.413083465285518,-0.05953,-0.993751811093549));
#7643=CARTESIAN_POINT('Origin',(0.,-0.05953,0.));
#7644=CARTESIAN_POINT('Origin',(0.685838782044607,-0.05953,-0.860014630714833));
#7645=CARTESIAN_POINT('Origin',(0.685838782044607,0.,-0.860014630714833));
#7646=CARTESIAN_POINT('',(0.876916659919095,-0.05953,-0.623857181492959));
#7647=CARTESIAN_POINT('Ctrl Pts',(0.876916659919095,-0.05953,-0.623857181492958));
#7648=CARTESIAN_POINT('Ctrl Pts',(0.873158080166742,-0.0925528133349865,
-0.62914037979579));
#7649=CARTESIAN_POINT('Ctrl Pts',(0.866144010579847,-0.124911173756694,
-0.638954437806245));
#7650=CARTESIAN_POINT('Ctrl Pts',(0.847641868610495,-0.177924977804098,
-0.663225258065736));
#7651=CARTESIAN_POINT('Ctrl Pts',(0.837310877969633,-0.199697230012983,
-0.676354402927683));
#7652=CARTESIAN_POINT('Ctrl Pts',(0.81280533416753,-0.237895043532788,-0.705614819529209));
#7653=CARTESIAN_POINT('Ctrl Pts',(0.798619410861634,-0.254319232363049,
-0.721738358858166));
#7654=CARTESIAN_POINT('Ctrl Pts',(0.768033796848072,-0.28018331644634,-0.754175290318038));
#7655=CARTESIAN_POINT('Ctrl Pts',(0.750136149454208,-0.29104845371857,-0.772120216227122));
#7656=CARTESIAN_POINT('Ctrl Pts',(0.711480111898423,-0.30527573347708,-0.807879894508811));
#7657=CARTESIAN_POINT('Ctrl Pts',(0.690705563850638,-0.308638795020976,
-0.825676810575913));
#7658=CARTESIAN_POINT('Ctrl Pts',(0.651278921914856,-0.308638795020976,
-0.857118508332695));
#7659=CARTESIAN_POINT('Ctrl Pts',(0.629305439856167,-0.30527573347708,-0.873412008702649));
#7660=CARTESIAN_POINT('Ctrl Pts',(0.585840553788742,-0.29104845371857,-0.903141581680914));
#7661=CARTESIAN_POINT('Ctrl Pts',(0.564362943424239,-0.28018331644634,-0.916597376014514));
#7662=CARTESIAN_POINT('Ctrl Pts',(0.525933334162556,-0.254319232363049,
-0.939198248544427));
#7663=CARTESIAN_POINT('Ctrl Pts',(0.507057380724533,-0.237895043532788,
-0.949440676105255));
#7664=CARTESIAN_POINT('Ctrl Pts',(0.473077587363686,-0.199697230012983,
-0.966820759530997));
#7665=CARTESIAN_POINT('Ctrl Pts',(0.457978755888596,-0.177924977804098,
-0.973971221090534));
#7666=CARTESIAN_POINT('Ctrl Pts',(0.430199341854858,-0.124911173756694,
-0.986608710139579));
#7667=CARTESIAN_POINT('Ctrl Pts',(0.419070565453384,-0.0925528133349865,
-0.991263089003441));
#7668=CARTESIAN_POINT('Ctrl Pts',(0.413083465285518,-0.05953,-0.993751811093549));
#7669=CARTESIAN_POINT('Origin',(0.685838782044607,-0.05953,-0.860014630714833));
#7670=CARTESIAN_POINT('Origin',(0.,-0.208355,0.));
#7671=CARTESIAN_POINT('',(-1.076188,-0.35718,1.31795018948079E-16));
#7672=CARTESIAN_POINT('Origin',(0.,-0.35718,0.));
#7673=CARTESIAN_POINT('',(-1.076188,-0.208355,1.31795018948079E-16));
#7674=CARTESIAN_POINT('',(1.03449977959455,-0.05953,0.296632461748266));
#7675=CARTESIAN_POINT('Origin',(0.,-0.05953,0.));
#7676=CARTESIAN_POINT('',(1.03449977959455,-0.05953,-0.296632461748266));
#7677=CARTESIAN_POINT('Ctrl Pts',(1.03449977959455,-0.05953,0.296632461748267));
#7678=CARTESIAN_POINT('Ctrl Pts',(1.03628691421076,-0.0925528133349865,
0.290399865505497));
#7679=CARTESIAN_POINT('Ctrl Pts',(1.03958665287714,-0.124911173756694,0.278797079997872));
#7680=CARTESIAN_POINT('Ctrl Pts',(1.0470264474309,-0.177924977804098,0.249198913998601));
#7681=CARTESIAN_POINT('Ctrl Pts',(1.05084995891418,-0.199697230012983,0.232935932341942));
#7682=CARTESIAN_POINT('Ctrl Pts',(1.05844771715377,-0.237895043532788,0.195533155353269));
#7683=CARTESIAN_POINT('Ctrl Pts',(1.06220882929878,-0.254319232363049,0.17438929156337));
#7684=CARTESIAN_POINT('Ctrl Pts',(1.06849922508772,-0.28018331644634,0.130252399648131));
#7685=CARTESIAN_POINT('Ctrl Pts',(1.07137013248666,-0.29104845371857,0.105070977154072));
#7686=CARTESIAN_POINT('Ctrl Pts',(1.07522652957392,-0.30527573347708,0.0525526752791107));
#7687=CARTESIAN_POINT('Ctrl Pts',(1.076188,-0.308638795020976,0.025214283908933));
#7688=CARTESIAN_POINT('Ctrl Pts',(1.076188,-0.308638795020976,-0.025214283908933));
#7689=CARTESIAN_POINT('Ctrl Pts',(1.07522652957392,-0.30527573347708,-0.0525526752791107));
#7690=CARTESIAN_POINT('Ctrl Pts',(1.07137013248666,-0.29104845371857,-0.105070977154072));
#7691=CARTESIAN_POINT('Ctrl Pts',(1.06849922508772,-0.28018331644634,-0.130252399648131));
#7692=CARTESIAN_POINT('Ctrl Pts',(1.06220882929878,-0.254319232363049,-0.17438929156337));
#7693=CARTESIAN_POINT('Ctrl Pts',(1.05844771715377,-0.237895043532788,-0.195533155353269));
#7694=CARTESIAN_POINT('Ctrl Pts',(1.05084995891418,-0.199697230012983,-0.232935932341942));
#7695=CARTESIAN_POINT('Ctrl Pts',(1.0470264474309,-0.177924977804098,-0.249198913998601));
#7696=CARTESIAN_POINT('Ctrl Pts',(1.03958665287714,-0.124911173756694,-0.278797079997872));
#7697=CARTESIAN_POINT('Ctrl Pts',(1.03628691421076,-0.0925528133349865,
-0.290399865505497));
#7698=CARTESIAN_POINT('Ctrl Pts',(1.03449977959455,-0.05953,-0.296632461748267));
#7699=CARTESIAN_POINT('Origin',(0.,-0.05953,0.));
#7700=CARTESIAN_POINT('Origin',(0.,-0.05953,0.));
#7701=CARTESIAN_POINT('Origin',(1.1,-0.05953,0.));
#7702=CARTESIAN_POINT('Origin',(1.1,0.,0.));
#7703=CARTESIAN_POINT('Origin',(1.1,-0.05953,0.));
#7704=CARTESIAN_POINT('Origin',(0.,-0.35718,0.));
#7705=CARTESIAN_POINT('Origin',(0.,-0.05953,0.));
#7706=CARTESIAN_POINT('',(0.,0.,0.));
#7707=CARTESIAN_POINT('Origin',(1.119765,0.495,0.));
#7708=CARTESIAN_POINT('',(-1.119765,0.495,-1.37131662304724E-16));
#7709=CARTESIAN_POINT('Origin',(0.,0.495,0.));
#7710=CARTESIAN_POINT('',(-1.085235,0.495,-1.32902956907268E-16));
#7711=CARTESIAN_POINT('Origin',(0.,0.495,0.));
#7712=CARTESIAN_POINT('Origin',(0.,0.4575,0.));
#7713=CARTESIAN_POINT('',(-1.119765,0.42,-1.37131662304724E-16));
#7714=CARTESIAN_POINT('Origin',(0.,0.42,0.));
#7715=CARTESIAN_POINT('',(-1.119765,0.4575,-1.37131662304724E-16));
#7716=CARTESIAN_POINT('Origin',(1.085235,0.42,0.));
#7717=CARTESIAN_POINT('',(-1.085235,0.42,-1.32902956907268E-16));
#7718=CARTESIAN_POINT('Origin',(0.,0.42,0.));
#7719=CARTESIAN_POINT('Origin',(0.,0.4575,0.));
#7720=CARTESIAN_POINT('',(-1.085235,0.4575,-1.32902956907268E-16));
#7721=CARTESIAN_POINT('Origin',(1.119765,-0.42,0.));
#7722=CARTESIAN_POINT('',(-1.119765,-0.42,-1.37131662304724E-16));
#7723=CARTESIAN_POINT('Origin',(0.,-0.42,0.));
#7724=CARTESIAN_POINT('',(-1.085235,-0.42,-1.32902956907268E-16));
#7725=CARTESIAN_POINT('Origin',(0.,-0.42,0.));
#7726=CARTESIAN_POINT('Origin',(0.,-0.4575,0.));
#7727=CARTESIAN_POINT('',(-1.119765,-0.495,-1.37131662304724E-16));
#7728=CARTESIAN_POINT('Origin',(0.,-0.495,0.));
#7729=CARTESIAN_POINT('',(-1.119765,-0.4575,-1.37131662304724E-16));
#7730=CARTESIAN_POINT('Origin',(1.085235,-0.495,0.));
#7731=CARTESIAN_POINT('',(-1.085235,-0.495,-1.32902956907268E-16));
#7732=CARTESIAN_POINT('Origin',(0.,-0.495,0.));
#7733=CARTESIAN_POINT('Origin',(0.,-0.4575,0.));
#7734=CARTESIAN_POINT('',(-1.085235,-0.4575,-1.32902956907268E-16));
#7735=CARTESIAN_POINT('',(0.,0.,0.));
#7736=CARTESIAN_POINT('',(0.,0.,0.));
#7737=CARTESIAN_POINT('',(0.,0.,0.));
#7738=CARTESIAN_POINT('',(0.,0.,0.));
#7739=CARTESIAN_POINT('',(0.,0.,0.));
#7740=CARTESIAN_POINT('',(0.,0.,0.));
#7741=CARTESIAN_POINT('Origin',(0.,1.1,3.5));
#7742=CARTESIAN_POINT('',(-1.2,1.3,3.5));
#7743=CARTESIAN_POINT('Origin',(0.,1.3,3.5));
#7744=CARTESIAN_POINT('',(-1.2,1.1,3.5));
#7745=CARTESIAN_POINT('',(-1.2,1.1,3.5));
#7746=CARTESIAN_POINT('Origin',(0.,1.1,3.5));
#7747=CARTESIAN_POINT('Origin',(0.,1.1,3.5));
#7748=CARTESIAN_POINT('',(-1.6,1.3,3.5));
#7749=CARTESIAN_POINT('Origin',(0.,1.3,3.5));
#7750=CARTESIAN_POINT('',(-1.6,1.1,3.5));
#7751=CARTESIAN_POINT('',(-1.6,1.1,3.5));
#7752=CARTESIAN_POINT('Origin',(0.,1.1,3.5));
#7753=CARTESIAN_POINT('Origin',(0.,1.3,3.5));
#7754=CARTESIAN_POINT('Origin',(0.,1.1,3.5));
#7755=CARTESIAN_POINT('',(0.,0.,0.));
#7756=CARTESIAN_POINT('',(0.,-0.6,4.));
#7757=CARTESIAN_POINT('',(0.,0.6,4.));
#7758=CARTESIAN_POINT('',(0.,0.,0.5));
#7759=CARTESIAN_POINT('',(0.,-2.4,0.5));
#7760=CARTESIAN_POINT('',(0.,0.,0.));
#7761=CARTESIAN_POINT('',(0.,0.,0.));
#7762=CARTESIAN_POINT('',(0.,0.,0.));
#7763=UNCERTAINTY_MEASURE_WITH_UNIT(LENGTH_MEASURE(0.001),#7817,
'DISTANCE_ACCURACY_VALUE',
'Maximum model space distance between geometric entities at asserted c
onnectivities');
#7764=UNCERTAINTY_MEASURE_WITH_UNIT(LENGTH_MEASURE(0.001),#7817,
'DISTANCE_ACCURACY_VALUE',
'Maximum model space distance between geometric entities at asserted c
onnectivities');
#7765=UNCERTAINTY_MEASURE_WITH_UNIT(LENGTH_MEASURE(0.001),#7817,
'DISTANCE_ACCURACY_VALUE',
'Maximum model space distance between geometric entities at asserted c
onnectivities');
#7766=UNCERTAINTY_MEASURE_WITH_UNIT(LENGTH_MEASURE(0.001),#7817,
'DISTANCE_ACCURACY_VALUE',
'Maximum model space distance between geometric entities at asserted c
onnectivities');
#7767=UNCERTAINTY_MEASURE_WITH_UNIT(LENGTH_MEASURE(0.001),#7817,
'DISTANCE_ACCURACY_VALUE',
'Maximum model space distance between geometric entities at asserted c
onnectivities');
#7768=UNCERTAINTY_MEASURE_WITH_UNIT(LENGTH_MEASURE(0.001),#7817,
'DISTANCE_ACCURACY_VALUE',
'Maximum model space distance between geometric entities at asserted c
onnectivities');
#7769=UNCERTAINTY_MEASURE_WITH_UNIT(LENGTH_MEASURE(0.001),#7817,
'DISTANCE_ACCURACY_VALUE',
'Maximum model space distance between geometric entities at asserted c
onnectivities');
#7770=UNCERTAINTY_MEASURE_WITH_UNIT(LENGTH_MEASURE(0.001),#7817,
'DISTANCE_ACCURACY_VALUE',
'Maximum model space distance between geometric entities at asserted c
onnectivities');
#7771=UNCERTAINTY_MEASURE_WITH_UNIT(LENGTH_MEASURE(0.001),#7817,
'DISTANCE_ACCURACY_VALUE',
'Maximum model space distance between geometric entities at asserted c
onnectivities');
#7772=UNCERTAINTY_MEASURE_WITH_UNIT(LENGTH_MEASURE(0.001),#7817,
'DISTANCE_ACCURACY_VALUE',
'Maximum model space distance between geometric entities at asserted c
onnectivities');
#7773=UNCERTAINTY_MEASURE_WITH_UNIT(LENGTH_MEASURE(0.001),#7817,
'DISTANCE_ACCURACY_VALUE',
'Maximum model space distance between geometric entities at asserted c
onnectivities');
#7774=UNCERTAINTY_MEASURE_WITH_UNIT(LENGTH_MEASURE(0.001),#7817,
'DISTANCE_ACCURACY_VALUE',
'Maximum model space distance between geometric entities at asserted c
onnectivities');
#7775=UNCERTAINTY_MEASURE_WITH_UNIT(LENGTH_MEASURE(0.001),#7817,
'DISTANCE_ACCURACY_VALUE',
'Maximum model space distance between geometric entities at asserted c
onnectivities');
#7776=UNCERTAINTY_MEASURE_WITH_UNIT(LENGTH_MEASURE(0.001),#7817,
'DISTANCE_ACCURACY_VALUE',
'Maximum model space distance between geometric entities at asserted c
onnectivities');
#7777=UNCERTAINTY_MEASURE_WITH_UNIT(LENGTH_MEASURE(0.001),#7817,
'DISTANCE_ACCURACY_VALUE',
'Maximum model space distance between geometric entities at asserted c
onnectivities');
#7778=UNCERTAINTY_MEASURE_WITH_UNIT(LENGTH_MEASURE(0.001),#7817,
'DISTANCE_ACCURACY_VALUE',
'Maximum model space distance between geometric entities at asserted c
onnectivities');
#7779=UNCERTAINTY_MEASURE_WITH_UNIT(LENGTH_MEASURE(0.001),#7817,
'DISTANCE_ACCURACY_VALUE',
'Maximum model space distance between geometric entities at asserted c
onnectivities');
#7780=UNCERTAINTY_MEASURE_WITH_UNIT(LENGTH_MEASURE(0.001),#7817,
'DISTANCE_ACCURACY_VALUE',
'Maximum model space distance between geometric entities at asserted c
onnectivities');
#7781=UNCERTAINTY_MEASURE_WITH_UNIT(LENGTH_MEASURE(0.001),#7817,
'DISTANCE_ACCURACY_VALUE',
'Maximum model space distance between geometric entities at asserted c
onnectivities');
#7782=UNCERTAINTY_MEASURE_WITH_UNIT(LENGTH_MEASURE(0.001),#7817,
'DISTANCE_ACCURACY_VALUE',
'Maximum model space distance between geometric entities at asserted c
onnectivities');
#7783=UNCERTAINTY_MEASURE_WITH_UNIT(LENGTH_MEASURE(0.001),#7817,
'DISTANCE_ACCURACY_VALUE',
'Maximum model space distance between geometric entities at asserted c
onnectivities');
#7784=UNCERTAINTY_MEASURE_WITH_UNIT(LENGTH_MEASURE(0.001),#7817,
'DISTANCE_ACCURACY_VALUE',
'Maximum model space distance between geometric entities at asserted c
onnectivities');
#7785=UNCERTAINTY_MEASURE_WITH_UNIT(LENGTH_MEASURE(0.001),#7817,
'DISTANCE_ACCURACY_VALUE',
'Maximum model space distance between geometric entities at asserted c
onnectivities');
#7786=UNCERTAINTY_MEASURE_WITH_UNIT(LENGTH_MEASURE(0.001),#7817,
'DISTANCE_ACCURACY_VALUE',
'Maximum model space distance between geometric entities at asserted c
onnectivities');
#7787=UNCERTAINTY_MEASURE_WITH_UNIT(LENGTH_MEASURE(0.001),#7817,
'DISTANCE_ACCURACY_VALUE',
'Maximum model space distance between geometric entities at asserted c
onnectivities');
#7788=UNCERTAINTY_MEASURE_WITH_UNIT(LENGTH_MEASURE(0.001),#7817,
'DISTANCE_ACCURACY_VALUE',
'Maximum model space distance between geometric entities at asserted c
onnectivities');
#7789=UNCERTAINTY_MEASURE_WITH_UNIT(LENGTH_MEASURE(0.001),#7817,
'DISTANCE_ACCURACY_VALUE',
'Maximum model space distance between geometric entities at asserted c
onnectivities');
#7790=(
GEOMETRIC_REPRESENTATION_CONTEXT(3)
GLOBAL_UNCERTAINTY_ASSIGNED_CONTEXT((#7763))
GLOBAL_UNIT_ASSIGNED_CONTEXT((#7817,#7819,#7820))
REPRESENTATION_CONTEXT('','3D')
);
#7791=(
GEOMETRIC_REPRESENTATION_CONTEXT(3)
GLOBAL_UNCERTAINTY_ASSIGNED_CONTEXT((#7764))
GLOBAL_UNIT_ASSIGNED_CONTEXT((#7817,#7819,#7820))
REPRESENTATION_CONTEXT('','3D')
);
#7792=(
GEOMETRIC_REPRESENTATION_CONTEXT(3)
GLOBAL_UNCERTAINTY_ASSIGNED_CONTEXT((#7765))
GLOBAL_UNIT_ASSIGNED_CONTEXT((#7817,#7819,#7820))
REPRESENTATION_CONTEXT('','3D')
);
#7793=(
GEOMETRIC_REPRESENTATION_CONTEXT(3)
GLOBAL_UNCERTAINTY_ASSIGNED_CONTEXT((#7766))
GLOBAL_UNIT_ASSIGNED_CONTEXT((#7817,#7819,#7820))
REPRESENTATION_CONTEXT('','3D')
);
#7794=(
GEOMETRIC_REPRESENTATION_CONTEXT(3)
GLOBAL_UNCERTAINTY_ASSIGNED_CONTEXT((#7767))
GLOBAL_UNIT_ASSIGNED_CONTEXT((#7817,#7819,#7820))
REPRESENTATION_CONTEXT('','3D')
);
#7795=(
GEOMETRIC_REPRESENTATION_CONTEXT(3)
GLOBAL_UNCERTAINTY_ASSIGNED_CONTEXT((#7768))
GLOBAL_UNIT_ASSIGNED_CONTEXT((#7817,#7819,#7820))
REPRESENTATION_CONTEXT('','3D')
);
#7796=(
GEOMETRIC_REPRESENTATION_CONTEXT(3)
GLOBAL_UNCERTAINTY_ASSIGNED_CONTEXT((#7769))
GLOBAL_UNIT_ASSIGNED_CONTEXT((#7817,#7819,#7820))
REPRESENTATION_CONTEXT('','3D')
);
#7797=(
GEOMETRIC_REPRESENTATION_CONTEXT(3)
GLOBAL_UNCERTAINTY_ASSIGNED_CONTEXT((#7770))
GLOBAL_UNIT_ASSIGNED_CONTEXT((#7817,#7819,#7820))
REPRESENTATION_CONTEXT('','3D')
);
#7798=(
GEOMETRIC_REPRESENTATION_CONTEXT(3)
GLOBAL_UNCERTAINTY_ASSIGNED_CONTEXT((#7771))
GLOBAL_UNIT_ASSIGNED_CONTEXT((#7817,#7819,#7820))
REPRESENTATION_CONTEXT('','3D')
);
#7799=(
GEOMETRIC_REPRESENTATION_CONTEXT(3)
GLOBAL_UNCERTAINTY_ASSIGNED_CONTEXT((#7772))
GLOBAL_UNIT_ASSIGNED_CONTEXT((#7817,#7819,#7820))
REPRESENTATION_CONTEXT('','3D')
);
#7800=(
GEOMETRIC_REPRESENTATION_CONTEXT(3)
GLOBAL_UNCERTAINTY_ASSIGNED_CONTEXT((#7773))
GLOBAL_UNIT_ASSIGNED_CONTEXT((#7817,#7819,#7820))
REPRESENTATION_CONTEXT('','3D')
);
#7801=(
GEOMETRIC_REPRESENTATION_CONTEXT(3)
GLOBAL_UNCERTAINTY_ASSIGNED_CONTEXT((#7774))
GLOBAL_UNIT_ASSIGNED_CONTEXT((#7817,#7819,#7820))
REPRESENTATION_CONTEXT('','3D')
);
#7802=(
GEOMETRIC_REPRESENTATION_CONTEXT(3)
GLOBAL_UNCERTAINTY_ASSIGNED_CONTEXT((#7775))
GLOBAL_UNIT_ASSIGNED_CONTEXT((#7817,#7819,#7820))
REPRESENTATION_CONTEXT('','3D')
);
#7803=(
GEOMETRIC_REPRESENTATION_CONTEXT(3)
GLOBAL_UNCERTAINTY_ASSIGNED_CONTEXT((#7776))
GLOBAL_UNIT_ASSIGNED_CONTEXT((#7817,#7819,#7820))
REPRESENTATION_CONTEXT('','3D')
);
#7804=(
GEOMETRIC_REPRESENTATION_CONTEXT(3)
GLOBAL_UNCERTAINTY_ASSIGNED_CONTEXT((#7777))
GLOBAL_UNIT_ASSIGNED_CONTEXT((#7817,#7819,#7820))
REPRESENTATION_CONTEXT('','3D')
);
#7805=(
GEOMETRIC_REPRESENTATION_CONTEXT(3)
GLOBAL_UNCERTAINTY_ASSIGNED_CONTEXT((#7778))
GLOBAL_UNIT_ASSIGNED_CONTEXT((#7817,#7819,#7820))
REPRESENTATION_CONTEXT('','3D')
);
#7806=(
GEOMETRIC_REPRESENTATION_CONTEXT(3)
GLOBAL_UNCERTAINTY_ASSIGNED_CONTEXT((#7779))
GLOBAL_UNIT_ASSIGNED_CONTEXT((#7817,#7819,#7820))
REPRESENTATION_CONTEXT('','3D')
);
#7807=(
GEOMETRIC_REPRESENTATION_CONTEXT(3)
GLOBAL_UNCERTAINTY_ASSIGNED_CONTEXT((#7780))
GLOBAL_UNIT_ASSIGNED_CONTEXT((#7817,#7819,#7820))
REPRESENTATION_CONTEXT('','3D')
);
#7808=(
GEOMETRIC_REPRESENTATION_CONTEXT(3)
GLOBAL_UNCERTAINTY_ASSIGNED_CONTEXT((#7781))
GLOBAL_UNIT_ASSIGNED_CONTEXT((#7817,#7819,#7820))
REPRESENTATION_CONTEXT('','3D')
);
#7809=(
GEOMETRIC_REPRESENTATION_CONTEXT(3)
GLOBAL_UNCERTAINTY_ASSIGNED_CONTEXT((#7782))
GLOBAL_UNIT_ASSIGNED_CONTEXT((#7817,#7819,#7820))
REPRESENTATION_CONTEXT('','3D')
);
#7810=(
GEOMETRIC_REPRESENTATION_CONTEXT(3)
GLOBAL_UNCERTAINTY_ASSIGNED_CONTEXT((#7783))
GLOBAL_UNIT_ASSIGNED_CONTEXT((#7817,#7819,#7820))
REPRESENTATION_CONTEXT('','3D')
);
#7811=(
GEOMETRIC_REPRESENTATION_CONTEXT(3)
GLOBAL_UNCERTAINTY_ASSIGNED_CONTEXT((#7784))
GLOBAL_UNIT_ASSIGNED_CONTEXT((#7817,#7819,#7820))
REPRESENTATION_CONTEXT('','3D')
);
#7812=(
GEOMETRIC_REPRESENTATION_CONTEXT(3)
GLOBAL_UNCERTAINTY_ASSIGNED_CONTEXT((#7785))
GLOBAL_UNIT_ASSIGNED_CONTEXT((#7817,#7819,#7820))
REPRESENTATION_CONTEXT('','3D')
);
#7813=(
GEOMETRIC_REPRESENTATION_CONTEXT(3)
GLOBAL_UNCERTAINTY_ASSIGNED_CONTEXT((#7786))
GLOBAL_UNIT_ASSIGNED_CONTEXT((#7817,#7819,#7820))
REPRESENTATION_CONTEXT('','3D')
);
#7814=(
GEOMETRIC_REPRESENTATION_CONTEXT(3)
GLOBAL_UNCERTAINTY_ASSIGNED_CONTEXT((#7787))
GLOBAL_UNIT_ASSIGNED_CONTEXT((#7817,#7819,#7820))
REPRESENTATION_CONTEXT('','3D')
);
#7815=(
GEOMETRIC_REPRESENTATION_CONTEXT(3)
GLOBAL_UNCERTAINTY_ASSIGNED_CONTEXT((#7788))
GLOBAL_UNIT_ASSIGNED_CONTEXT((#7817,#7819,#7820))
REPRESENTATION_CONTEXT('','3D')
);
#7816=(
GEOMETRIC_REPRESENTATION_CONTEXT(3)
GLOBAL_UNCERTAINTY_ASSIGNED_CONTEXT((#7789))
GLOBAL_UNIT_ASSIGNED_CONTEXT((#7817,#7819,#7820))
REPRESENTATION_CONTEXT('','3D')
);
#7817=(
LENGTH_UNIT()
NAMED_UNIT(*)
SI_UNIT(.CENTI.,.METRE.)
);
#7818=(
LENGTH_UNIT()
NAMED_UNIT(*)
SI_UNIT($,.METRE.)
);
#7819=(
NAMED_UNIT(*)
PLANE_ANGLE_UNIT()
SI_UNIT($,.RADIAN.)
);
#7820=(
NAMED_UNIT(*)
SI_UNIT($,.STERADIAN.)
SOLID_ANGLE_UNIT()
);
#7821=SHAPE_DEFINITION_REPRESENTATION(#7847,#7901);
#7822=SHAPE_DEFINITION_REPRESENTATION(#7848,#7902);
#7823=SHAPE_DEFINITION_REPRESENTATION(#7849,#7903);
#7824=SHAPE_DEFINITION_REPRESENTATION(#7850,#7904);
#7825=SHAPE_DEFINITION_REPRESENTATION(#7851,#7905);
#7826=SHAPE_DEFINITION_REPRESENTATION(#7852,#7906);
#7827=SHAPE_DEFINITION_REPRESENTATION(#7853,#7907);
#7828=SHAPE_DEFINITION_REPRESENTATION(#7854,#7908);
#7829=SHAPE_DEFINITION_REPRESENTATION(#7858,#7909);
#7830=SHAPE_DEFINITION_REPRESENTATION(#7859,#7910);
#7831=SHAPE_DEFINITION_REPRESENTATION(#7865,#7911);
#7832=SHAPE_DEFINITION_REPRESENTATION(#7866,#7912);
#7833=SHAPE_DEFINITION_REPRESENTATION(#7867,#7913);
#7834=SHAPE_DEFINITION_REPRESENTATION(#7868,#7914);
#7835=SHAPE_DEFINITION_REPRESENTATION(#7869,#7915);
#7836=SHAPE_DEFINITION_REPRESENTATION(#7870,#7916);
#7837=SHAPE_DEFINITION_REPRESENTATION(#7871,#7917);
#7838=SHAPE_DEFINITION_REPRESENTATION(#7879,#7918);
#7839=SHAPE_DEFINITION_REPRESENTATION(#7880,#7919);
#7840=SHAPE_DEFINITION_REPRESENTATION(#7881,#7920);
#7841=SHAPE_DEFINITION_REPRESENTATION(#7882,#7921);
#7842=SHAPE_DEFINITION_REPRESENTATION(#7883,#7922);
#7843=SHAPE_DEFINITION_REPRESENTATION(#7884,#7923);
#7844=SHAPE_DEFINITION_REPRESENTATION(#7885,#7924);
#7845=SHAPE_DEFINITION_REPRESENTATION(#7886,#7925);
#7846=SHAPE_DEFINITION_REPRESENTATION(#7892,#7926);
#7847=PRODUCT_DEFINITION_SHAPE('',$,#7928);
#7848=PRODUCT_DEFINITION_SHAPE('',$,#7929);
#7849=PRODUCT_DEFINITION_SHAPE('',$,#7930);
#7850=PRODUCT_DEFINITION_SHAPE('',$,#7931);
#7851=PRODUCT_DEFINITION_SHAPE('',$,#7932);
#7852=PRODUCT_DEFINITION_SHAPE('',$,#7933);
#7853=PRODUCT_DEFINITION_SHAPE('',$,#7934);
#7854=PRODUCT_DEFINITION_SHAPE('',$,#7935);
#7855=PRODUCT_DEFINITION_SHAPE($,$,#118);
#7856=PRODUCT_DEFINITION_SHAPE($,$,#119);
#7857=PRODUCT_DEFINITION_SHAPE($,$,#120);
#7858=PRODUCT_DEFINITION_SHAPE('',$,#7936);
#7859=PRODUCT_DEFINITION_SHAPE('',$,#7937);
#7860=PRODUCT_DEFINITION_SHAPE($,$,#121);
#7861=PRODUCT_DEFINITION_SHAPE($,$,#122);
#7862=PRODUCT_DEFINITION_SHAPE($,$,#123);
#7863=PRODUCT_DEFINITION_SHAPE($,$,#124);
#7864=PRODUCT_DEFINITION_SHAPE($,$,#125);
#7865=PRODUCT_DEFINITION_SHAPE('',$,#7938);
#7866=PRODUCT_DEFINITION_SHAPE('',$,#7939);
#7867=PRODUCT_DEFINITION_SHAPE('',$,#7940);
#7868=PRODUCT_DEFINITION_SHAPE('',$,#7941);
#7869=PRODUCT_DEFINITION_SHAPE('',$,#7942);
#7870=PRODUCT_DEFINITION_SHAPE('',$,#7943);
#7871=PRODUCT_DEFINITION_SHAPE('',$,#7944);
#7872=PRODUCT_DEFINITION_SHAPE($,$,#126);
#7873=PRODUCT_DEFINITION_SHAPE($,$,#127);
#7874=PRODUCT_DEFINITION_SHAPE($,$,#128);
#7875=PRODUCT_DEFINITION_SHAPE($,$,#129);
#7876=PRODUCT_DEFINITION_SHAPE($,$,#130);
#7877=PRODUCT_DEFINITION_SHAPE($,$,#131);
#7878=PRODUCT_DEFINITION_SHAPE($,$,#132);
#7879=PRODUCT_DEFINITION_SHAPE('',$,#7945);
#7880=PRODUCT_DEFINITION_SHAPE('',$,#7946);
#7881=PRODUCT_DEFINITION_SHAPE('',$,#7947);
#7882=PRODUCT_DEFINITION_SHAPE('',$,#7948);
#7883=PRODUCT_DEFINITION_SHAPE('',$,#7949);
#7884=PRODUCT_DEFINITION_SHAPE('',$,#7950);
#7885=PRODUCT_DEFINITION_SHAPE('',$,#7951);
#7886=PRODUCT_DEFINITION_SHAPE('',$,#7952);
#7887=PRODUCT_DEFINITION_SHAPE($,$,#133);
#7888=PRODUCT_DEFINITION_SHAPE($,$,#134);
#7889=PRODUCT_DEFINITION_SHAPE($,$,#135);
#7890=PRODUCT_DEFINITION_SHAPE($,$,#136);
#7891=PRODUCT_DEFINITION_SHAPE($,$,#137);
#7892=PRODUCT_DEFINITION_SHAPE('',$,#7953);
#7893=PRODUCT_DEFINITION_SHAPE($,$,#138);
#7894=PRODUCT_DEFINITION_SHAPE($,$,#139);
#7895=PRODUCT_DEFINITION_SHAPE($,$,#140);
#7896=PRODUCT_DEFINITION_SHAPE($,$,#141);
#7897=PRODUCT_DEFINITION_SHAPE($,$,#142);
#7898=PRODUCT_DEFINITION_SHAPE($,$,#143);
#7899=PRODUCT_DEFINITION_SHAPE($,$,#144);
#7900=PRODUCT_DEFINITION_SHAPE($,$,#145);
#7901=SHAPE_REPRESENTATION('',(#3962,#4486,#4487,#4488),#7790);
#7902=SHAPE_REPRESENTATION('',(#3963,#4222,#4223,#4224,#4225,#4226),#7791);
#7903=SHAPE_REPRESENTATION('',(#3964),#7792);
#7904=SHAPE_REPRESENTATION('',(#3986),#7793);
#7905=SHAPE_REPRESENTATION('',(#4004,#4194,#4195,#4196),#7794);
#7906=SHAPE_REPRESENTATION('',(#4005),#7795);
#7907=SHAPE_REPRESENTATION('',(#4089),#7796);
#7908=SHAPE_REPRESENTATION('',(#4173),#7797);
#7909=SHAPE_REPRESENTATION('',(#4197),#7798);
#7910=SHAPE_REPRESENTATION('',(#4206),#7799);
#7911=SHAPE_REPRESENTATION('',(#4227,#4319,#4320,#4321,#4322,#4323,#4324,
#4325),#7800);
#7912=SHAPE_REPRESENTATION('',(#4228),#7801);
#7913=SHAPE_REPRESENTATION('',(#4254),#7802);
#7914=SHAPE_REPRESENTATION('',(#4263),#7803);
#7915=SHAPE_REPRESENTATION('',(#4277),#7804);
#7916=SHAPE_REPRESENTATION('',(#4286),#7805);
#7917=SHAPE_REPRESENTATION('',(#4295),#7806);
#7918=SHAPE_REPRESENTATION('',(#4326,#4481,#4482,#4483,#4484,#4485),#7807);
#7919=SHAPE_REPRESENTATION('',(#4327),#7808);
#7920=SHAPE_REPRESENTATION('',(#4344,#4467,#4468,#4469,#4470,#4471),#7809);
#7921=SHAPE_REPRESENTATION('',(#4345),#7810);
#7922=SHAPE_REPRESENTATION('',(#4365),#7811);
#7923=SHAPE_REPRESENTATION('',(#4385),#7812);
#7924=SHAPE_REPRESENTATION('',(#4400),#7813);
#7925=SHAPE_REPRESENTATION('',(#4450),#7814);
#7926=SHAPE_REPRESENTATION('',(#4472),#7815);
#7927=PRODUCT_DEFINITION_CONTEXT('part definition',#8007,'design');
#7928=PRODUCT_DEFINITION('PAT-005',
'PAT-005',#7954,#7927);
#7929=PRODUCT_DEFINITION('Mounting plate kingpin and ball race',
'Mounting plate kingpin and ball race',#7955,#7927);
#7930=PRODUCT_DEFINITION('Hundred by eighty mounting plate',
'Hundred by eighty mounting plate',#7956,#7927);
#7931=PRODUCT_DEFINITION('Stepped swivel kingpin',
'Stepped swivel kingpin',#7957,#7927);
#7932=PRODUCT_DEFINITION('Thrust Ball Bearing - 15 x 28 x 9 mm',
'Thrust Ball Bearing - 15 x 28 x 9 mm',#7958,#7927);
#7933=PRODUCT_DEFINITION('Shaft washer','Shaft washer',#7959,#7927);
#7934=PRODUCT_DEFINITION('Housing washer','Housing washer',#7960,#7927);
#7935=PRODUCT_DEFINITION('Balls','Balls',#7961,#7927);
#7936=PRODUCT_DEFINITION('Flat Washer - M8','Flat Washer - M8',#7962,#7927);
#7937=PRODUCT_DEFINITION('Hex Nut - M8','Hex Nut - M8',#7963,#7927);
#7938=PRODUCT_DEFINITION('Swivelling fork and dead axle',
'Swivelling fork and dead axle',#7964,#7927);
#7939=PRODUCT_DEFINITION('Twelve millimetre axle fork',
'Twelve millimetre axle fork',#7965,#7927);
#7940=PRODUCT_DEFINITION('Swivel bushing','Swivel bushing',#7966,#7927);
#7941=PRODUCT_DEFINITION('Twelve millimetre dead axle',
'Twelve millimetre dead axle',#7967,#7927);
#7942=PRODUCT_DEFINITION('Inner race spacer','Inner race spacer',#7968,
#7927);
#7943=PRODUCT_DEFINITION('Axle keeper','Axle keeper',#7969,#7927);
#7944=PRODUCT_DEFINITION('M4x10 Cap Screw','M4x10 Cap Screw',#7970,#7927);
#7945=PRODUCT_DEFINITION('Seventy-five millimetre wheel',
'Seventy-five millimetre wheel',#7971,#7927);
#7946=PRODUCT_DEFINITION('Wheel with twelve millimetre bearings',
'Wheel with twelve millimetre bearings',#7972,#7927);
#7947=PRODUCT_DEFINITION('Sealed Ball Bearing - 12 x 32 x 10 mm',
'Sealed Ball Bearing - 12 x 32 x 10 mm',#7973,#7927);
#7948=PRODUCT_DEFINITION('Inner ring','Inner ring',#7974,#7927);
#7949=PRODUCT_DEFINITION('Outer ring','Outer ring',#7975,#7927);
#7950=PRODUCT_DEFINITION('Balls (1)','Balls (1)',#7976,#7927);
#7951=PRODUCT_DEFINITION('Cage (1)','Cage (1)',#7977,#7927);
#7952=PRODUCT_DEFINITION('Seals 2RS','Seals 2RS',#7978,#7927);
#7953=PRODUCT_DEFINITION('Bearing end retainer','Bearing end retainer',
#7979,#7927);
#7954=PRODUCT_DEFINITION_FORMATION('',$,#8009);
#7955=PRODUCT_DEFINITION_FORMATION('',$,#8010);
#7956=PRODUCT_DEFINITION_FORMATION('',$,#8011);
#7957=PRODUCT_DEFINITION_FORMATION('',$,#8012);
#7958=PRODUCT_DEFINITION_FORMATION('',$,#8013);
#7959=PRODUCT_DEFINITION_FORMATION('',$,#8014);
#7960=PRODUCT_DEFINITION_FORMATION('',$,#8015);
#7961=PRODUCT_DEFINITION_FORMATION('',$,#8016);
#7962=PRODUCT_DEFINITION_FORMATION('',$,#8017);
#7963=PRODUCT_DEFINITION_FORMATION('',$,#8018);
#7964=PRODUCT_DEFINITION_FORMATION('',$,#8019);
#7965=PRODUCT_DEFINITION_FORMATION('',$,#8020);
#7966=PRODUCT_DEFINITION_FORMATION('',$,#8021);
#7967=PRODUCT_DEFINITION_FORMATION('',$,#8022);
#7968=PRODUCT_DEFINITION_FORMATION('',$,#8023);
#7969=PRODUCT_DEFINITION_FORMATION('',$,#8024);
#7970=PRODUCT_DEFINITION_FORMATION('',$,#8025);
#7971=PRODUCT_DEFINITION_FORMATION('',$,#8026);
#7972=PRODUCT_DEFINITION_FORMATION('',$,#8027);
#7973=PRODUCT_DEFINITION_FORMATION('',$,#8028);
#7974=PRODUCT_DEFINITION_FORMATION('',$,#8029);
#7975=PRODUCT_DEFINITION_FORMATION('',$,#8030);
#7976=PRODUCT_DEFINITION_FORMATION('',$,#8031);
#7977=PRODUCT_DEFINITION_FORMATION('',$,#8032);
#7978=PRODUCT_DEFINITION_FORMATION('',$,#8033);
#7979=PRODUCT_DEFINITION_FORMATION('',$,#8034);
#7980=PRODUCT_RELATED_PRODUCT_CATEGORY('PAT-005',
'PAT-005',(#8009));
#7981=PRODUCT_RELATED_PRODUCT_CATEGORY(
'Mounting plate kingpin and ball race',
'Mounting plate kingpin and ball race',(#8010));
#7982=PRODUCT_RELATED_PRODUCT_CATEGORY(
'Hundred by eighty mounting plate','Hundred by eighty mounting plate',(#8011));
#7983=PRODUCT_RELATED_PRODUCT_CATEGORY('Stepped swivel kingpin',
'Stepped swivel kingpin',(#8012));
#7984=PRODUCT_RELATED_PRODUCT_CATEGORY(
'Thrust Ball Bearing - 15 x 28 x 9 mm',
'Thrust Ball Bearing - 15 x 28 x 9 mm',(#8013));
#7985=PRODUCT_RELATED_PRODUCT_CATEGORY('Shaft washer','Shaft washer',(#8014));
#7986=PRODUCT_RELATED_PRODUCT_CATEGORY('Housing washer',
'Housing washer',(#8015));
#7987=PRODUCT_RELATED_PRODUCT_CATEGORY('Balls','Balls',(#8016));
#7988=PRODUCT_RELATED_PRODUCT_CATEGORY('Flat Washer - M8',
'Flat Washer - M8',(#8017));
#7989=PRODUCT_RELATED_PRODUCT_CATEGORY('Hex Nut - M8','Hex Nut - M8',(#8018));
#7990=PRODUCT_RELATED_PRODUCT_CATEGORY('Swivelling fork and dead axle',
'Swivelling fork and dead axle',(#8019));
#7991=PRODUCT_RELATED_PRODUCT_CATEGORY('Twelve millimetre axle fork',
'Twelve millimetre axle fork',(#8020));
#7992=PRODUCT_RELATED_PRODUCT_CATEGORY('Swivel bushing',
'Swivel bushing',(#8021));
#7993=PRODUCT_RELATED_PRODUCT_CATEGORY('Twelve millimetre dead axle',
'Twelve millimetre dead axle',(#8022));
#7994=PRODUCT_RELATED_PRODUCT_CATEGORY('Inner race spacer',
'Inner race spacer',(#8023));
#7995=PRODUCT_RELATED_PRODUCT_CATEGORY('Axle keeper','Axle keeper',(#8024));
#7996=PRODUCT_RELATED_PRODUCT_CATEGORY('M4x10 Cap Screw',
'M4x10 Cap Screw',(#8025));
#7997=PRODUCT_RELATED_PRODUCT_CATEGORY('Seventy-five millimetre wheel',
'Seventy-five millimetre wheel',(#8026));
#7998=PRODUCT_RELATED_PRODUCT_CATEGORY(
'Wheel with twelve millimetre bearings',
'Wheel with twelve millimetre bearings',(#8027));
#7999=PRODUCT_RELATED_PRODUCT_CATEGORY(
'Sealed Ball Bearing - 12 x 32 x 10 mm',
'Sealed Ball Bearing - 12 x 32 x 10 mm',(#8028));
#8000=PRODUCT_RELATED_PRODUCT_CATEGORY('Inner ring','Inner ring',(#8029));
#8001=PRODUCT_RELATED_PRODUCT_CATEGORY('Outer ring','Outer ring',(#8030));
#8002=PRODUCT_RELATED_PRODUCT_CATEGORY('Balls (1)','Balls (1)',(#8031));
#8003=PRODUCT_RELATED_PRODUCT_CATEGORY('Cage (1)','Cage (1)',(#8032));
#8004=PRODUCT_RELATED_PRODUCT_CATEGORY('Seals 2RS','Seals 2RS',(#8033));
#8005=PRODUCT_RELATED_PRODUCT_CATEGORY('Bearing end retainer',
'Bearing end retainer',(#8034));
#8006=APPLICATION_PROTOCOL_DEFINITION('international standard',
'automotive_design',2009,#8007);
#8007=APPLICATION_CONTEXT(
'Core Data for Automotive Mechanical Design Process');
#8008=PRODUCT_CONTEXT('part definition',#8007,'mechanical');
#8009=PRODUCT('PAT-005','PAT-005',
'PAT-005',(#8008));
#8010=PRODUCT('Mounting plate kingpin and ball race',
'Mounting plate kingpin and ball race',
'Mounting plate kingpin and ball race',(#8008));
#8011=PRODUCT('Hundred by eighty mounting plate',
'Hundred by eighty mounting plate','Hundred by eighty mounting plate',(#8008));
#8012=PRODUCT('Stepped swivel kingpin','Stepped swivel kingpin',
'Stepped swivel kingpin',(#8008));
#8013=PRODUCT('Thrust Ball Bearing - 15 x 28 x 9 mm',
'Thrust Ball Bearing - 15 x 28 x 9 mm',
'Thrust Ball Bearing - 15 x 28 x 9 mm',(#8008));
#8014=PRODUCT('Shaft washer','Shaft washer','Shaft washer',(#8008));
#8015=PRODUCT('Housing washer','Housing washer','Housing washer',(#8008));
#8016=PRODUCT('Balls','Balls','Balls',(#8008));
#8017=PRODUCT('Flat Washer - M8','Flat Washer - M8','Flat Washer - M8',
(#8008));
#8018=PRODUCT('Hex Nut - M8','Hex Nut - M8','Hex Nut - M8',(#8008));
#8019=PRODUCT('Swivelling fork and dead axle',
'Swivelling fork and dead axle','Swivelling fork and dead axle',(#8008));
#8020=PRODUCT('Twelve millimetre axle fork',
'Twelve millimetre axle fork','Twelve millimetre axle fork',(#8008));
#8021=PRODUCT('Swivel bushing','Swivel bushing','Swivel bushing',(#8008));
#8022=PRODUCT('Twelve millimetre dead axle',
'Twelve millimetre dead axle','Twelve millimetre dead axle',(#8008));
#8023=PRODUCT('Inner race spacer','Inner race spacer',
'Inner race spacer',(#8008));
#8024=PRODUCT('Axle keeper','Axle keeper','Axle keeper',(#8008));
#8025=PRODUCT('M4x10 Cap Screw','M4x10 Cap Screw','M4x10 Cap Screw',(#8008));
#8026=PRODUCT('Seventy-five millimetre wheel',
'Seventy-five millimetre wheel','Seventy-five millimetre wheel',(#8008));
#8027=PRODUCT('Wheel with twelve millimetre bearings',
'Wheel with twelve millimetre bearings',
'Wheel with twelve millimetre bearings',(#8008));
#8028=PRODUCT('Sealed Ball Bearing - 12 x 32 x 10 mm',
'Sealed Ball Bearing - 12 x 32 x 10 mm',
'Sealed Ball Bearing - 12 x 32 x 10 mm',(#8008));
#8029=PRODUCT('Inner ring','Inner ring','Inner ring',(#8008));
#8030=PRODUCT('Outer ring','Outer ring','Outer ring',(#8008));
#8031=PRODUCT('Balls (1)','Balls (1)','Balls (1)',(#8008));
#8032=PRODUCT('Cage (1)','Cage (1)','Cage (1)',(#8008));
#8033=PRODUCT('Seals 2RS','Seals 2RS','Seals 2RS',(#8008));
#8034=PRODUCT('Bearing end retainer','Bearing end retainer',
'Bearing end retainer',(#8008));
#8035=PRESENTATION_STYLE_ASSIGNMENT((#8040));
#8036=PRESENTATION_STYLE_ASSIGNMENT((#8041));
#8037=PRESENTATION_STYLE_ASSIGNMENT((#8042));
#8038=PRESENTATION_STYLE_ASSIGNMENT((#8043));
#8039=PRESENTATION_STYLE_ASSIGNMENT((#8044));
#8040=SURFACE_STYLE_USAGE(.BOTH.,#8045);
#8041=SURFACE_STYLE_USAGE(.BOTH.,#8046);
#8042=SURFACE_STYLE_USAGE(.BOTH.,#8047);
#8043=SURFACE_STYLE_USAGE(.BOTH.,#8048);
#8044=SURFACE_STYLE_USAGE(.BOTH.,#8049);
#8045=SURFACE_SIDE_STYLE('',(#8050));
#8046=SURFACE_SIDE_STYLE('',(#8051));
#8047=SURFACE_SIDE_STYLE('',(#8052));
#8048=SURFACE_SIDE_STYLE('',(#8053));
#8049=SURFACE_SIDE_STYLE('',(#8054));
#8050=SURFACE_STYLE_FILL_AREA(#8055);
#8051=SURFACE_STYLE_FILL_AREA(#8056);
#8052=SURFACE_STYLE_FILL_AREA(#8057);
#8053=SURFACE_STYLE_FILL_AREA(#8058);
#8054=SURFACE_STYLE_FILL_AREA(#8059);
#8055=FILL_AREA_STYLE('Steel - Satin',(#8060));
#8056=FILL_AREA_STYLE('CAD Library Painted - Engineering blue',(#8061));
#8057=FILL_AREA_STYLE('CAD Library Painted - Steel gray',(#8062));
#8058=FILL_AREA_STYLE('CAD Library Painted - Graphite',(#8063));
#8059=FILL_AREA_STYLE('CAD Library Painted - Off white',(#8064));
#8060=FILL_AREA_STYLE_COLOUR('Steel - Satin',#8065);
#8061=FILL_AREA_STYLE_COLOUR('CAD Library Painted - Engineering blue',#8066);
#8062=FILL_AREA_STYLE_COLOUR('CAD Library Painted - Steel gray',#8067);
#8063=FILL_AREA_STYLE_COLOUR('CAD Library Painted - Graphite',#8068);
#8064=FILL_AREA_STYLE_COLOUR('CAD Library Painted - Off white',#8069);
#8065=COLOUR_RGB('Steel - Satin',0.627450980392157,0.627450980392157,0.627450980392157);
#8066=COLOUR_RGB('CAD Library Painted - Engineering blue',0.12156862745098,
0.356862745098039,0.6);
#8067=COLOUR_RGB('CAD Library Painted - Steel gray',0.592156862745098,0.631372549019608,
0.67843137254902);
#8068=COLOUR_RGB('CAD Library Painted - Graphite',0.0980392156862745,0.109803921568627,
0.125490196078431);
#8069=COLOUR_RGB('CAD Library Painted - Off white',0.909803921568627,0.901960784313726,
0.858823529411765);
#8070=COLOUR_RGB('Dark Blue',0.08,0.2,0.34);
#8071=FILL_AREA_STYLE_COLOUR('',#8070);
#8072=FILL_AREA_STYLE('',(#8071));
#8073=SURFACE_STYLE_FILL_AREA(#8072);
#8074=SURFACE_SIDE_STYLE('',(#8073));
#8075=SURFACE_STYLE_USAGE(.BOTH.,#8074);
#8076=PRESENTATION_STYLE_ASSIGNMENT((#8075));
#8077=COLOUR_RGB('Light Blue',0.38,0.62,0.78);
#8078=FILL_AREA_STYLE_COLOUR('',#8077);
#8079=FILL_AREA_STYLE('',(#8078));
#8080=SURFACE_STYLE_FILL_AREA(#8079);
#8081=SURFACE_SIDE_STYLE('',(#8080));
#8082=SURFACE_STYLE_USAGE(.BOTH.,#8081);
#8083=PRESENTATION_STYLE_ASSIGNMENT((#8082));
#8084=COLOUR_RGB('Sky Blue',0.24,0.69,0.87);
#8085=FILL_AREA_STYLE_COLOUR('',#8084);
#8086=FILL_AREA_STYLE('',(#8085));
#8087=SURFACE_STYLE_FILL_AREA(#8086);
#8088=SURFACE_SIDE_STYLE('',(#8087));
#8089=SURFACE_STYLE_USAGE(.BOTH.,#8088);
#8090=PRESENTATION_STYLE_ASSIGNMENT((#8089));
#8091=COLOUR_RGB('Grey',0.48,0.52,0.57);
#8092=FILL_AREA_STYLE_COLOUR('',#8091);
#8093=FILL_AREA_STYLE('',(#8092));
#8094=SURFACE_STYLE_FILL_AREA(#8093);
#8095=SURFACE_SIDE_STYLE('',(#8094));
#8096=SURFACE_STYLE_USAGE(.BOTH.,#8095);
#8097=PRESENTATION_STYLE_ASSIGNMENT((#8096));
#8098=COLOUR_RGB('Black',0.12,0.14,0.17);
#8099=FILL_AREA_STYLE_COLOUR('',#8098);
#8100=FILL_AREA_STYLE('',(#8099));
#8101=SURFACE_STYLE_FILL_AREA(#8100);
#8102=SURFACE_SIDE_STYLE('',(#8101));
#8103=SURFACE_STYLE_USAGE(.BOTH.,#8102);
#8104=PRESENTATION_STYLE_ASSIGNMENT((#8103));
#8105=COLOUR_RGB('Off White',0.89,0.88,0.83);
#8106=FILL_AREA_STYLE_COLOUR('',#8105);
#8107=FILL_AREA_STYLE('',(#8106));
#8108=SURFACE_STYLE_FILL_AREA(#8107);
#8109=SURFACE_SIDE_STYLE('',(#8108));
#8110=SURFACE_STYLE_USAGE(.BOTH.,#8109);
#8111=PRESENTATION_STYLE_ASSIGNMENT((#8110));
ENDSEC;
END-ISO-10303-21;
